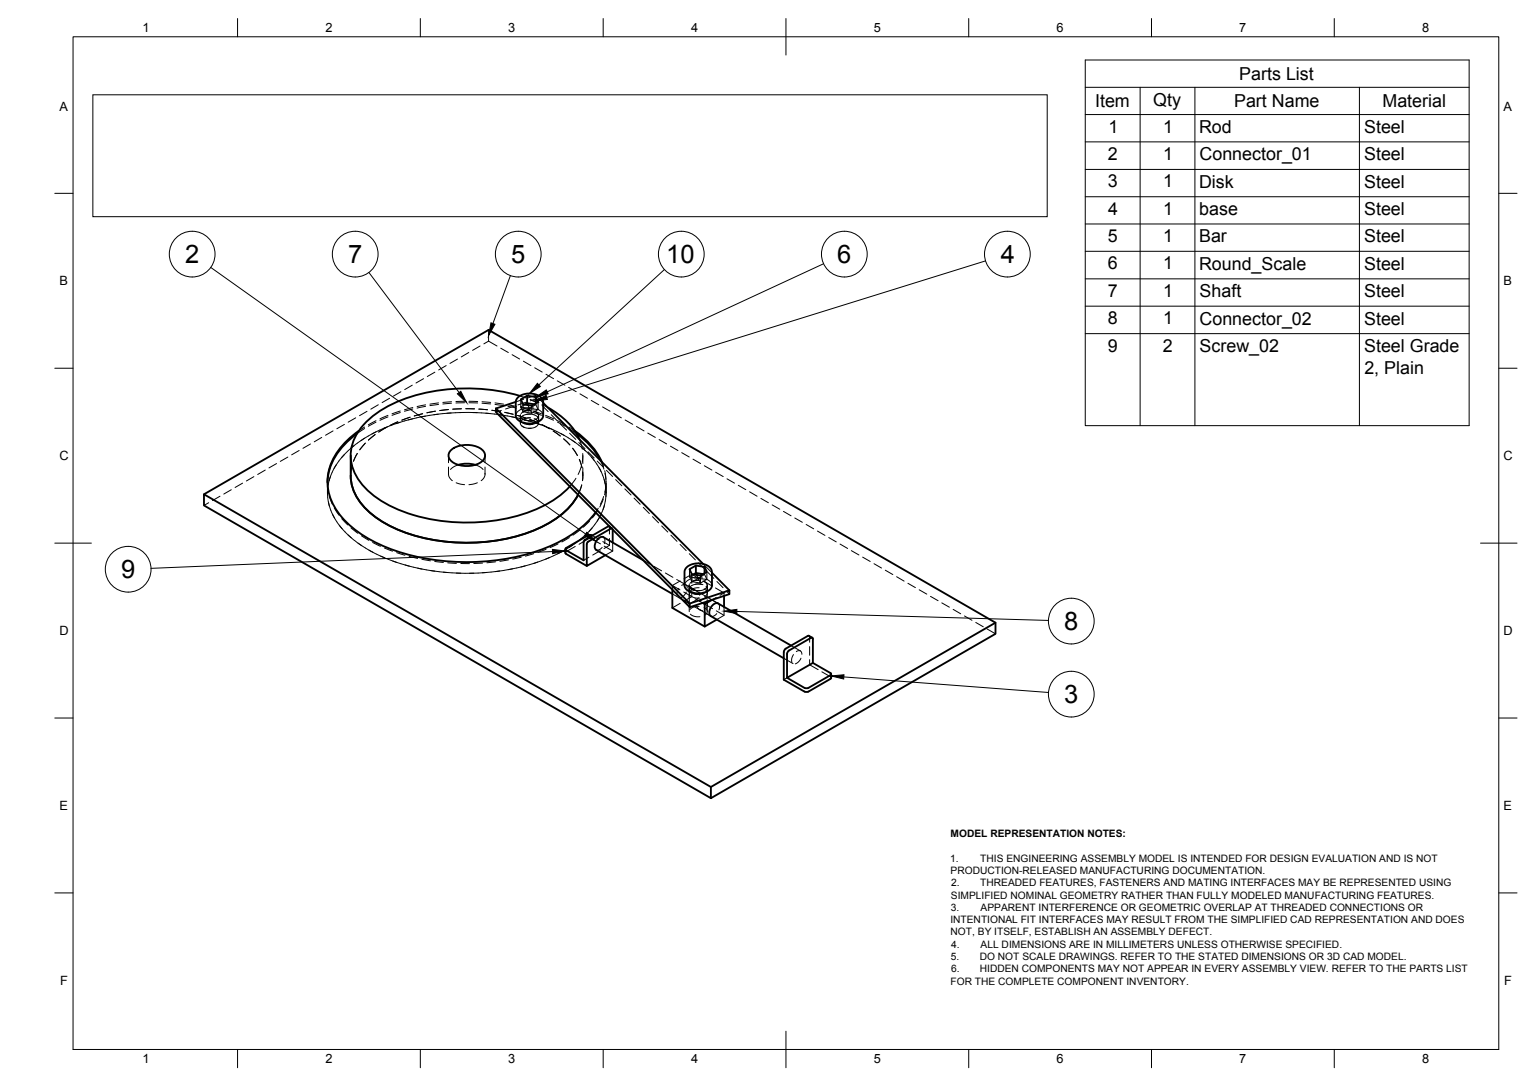
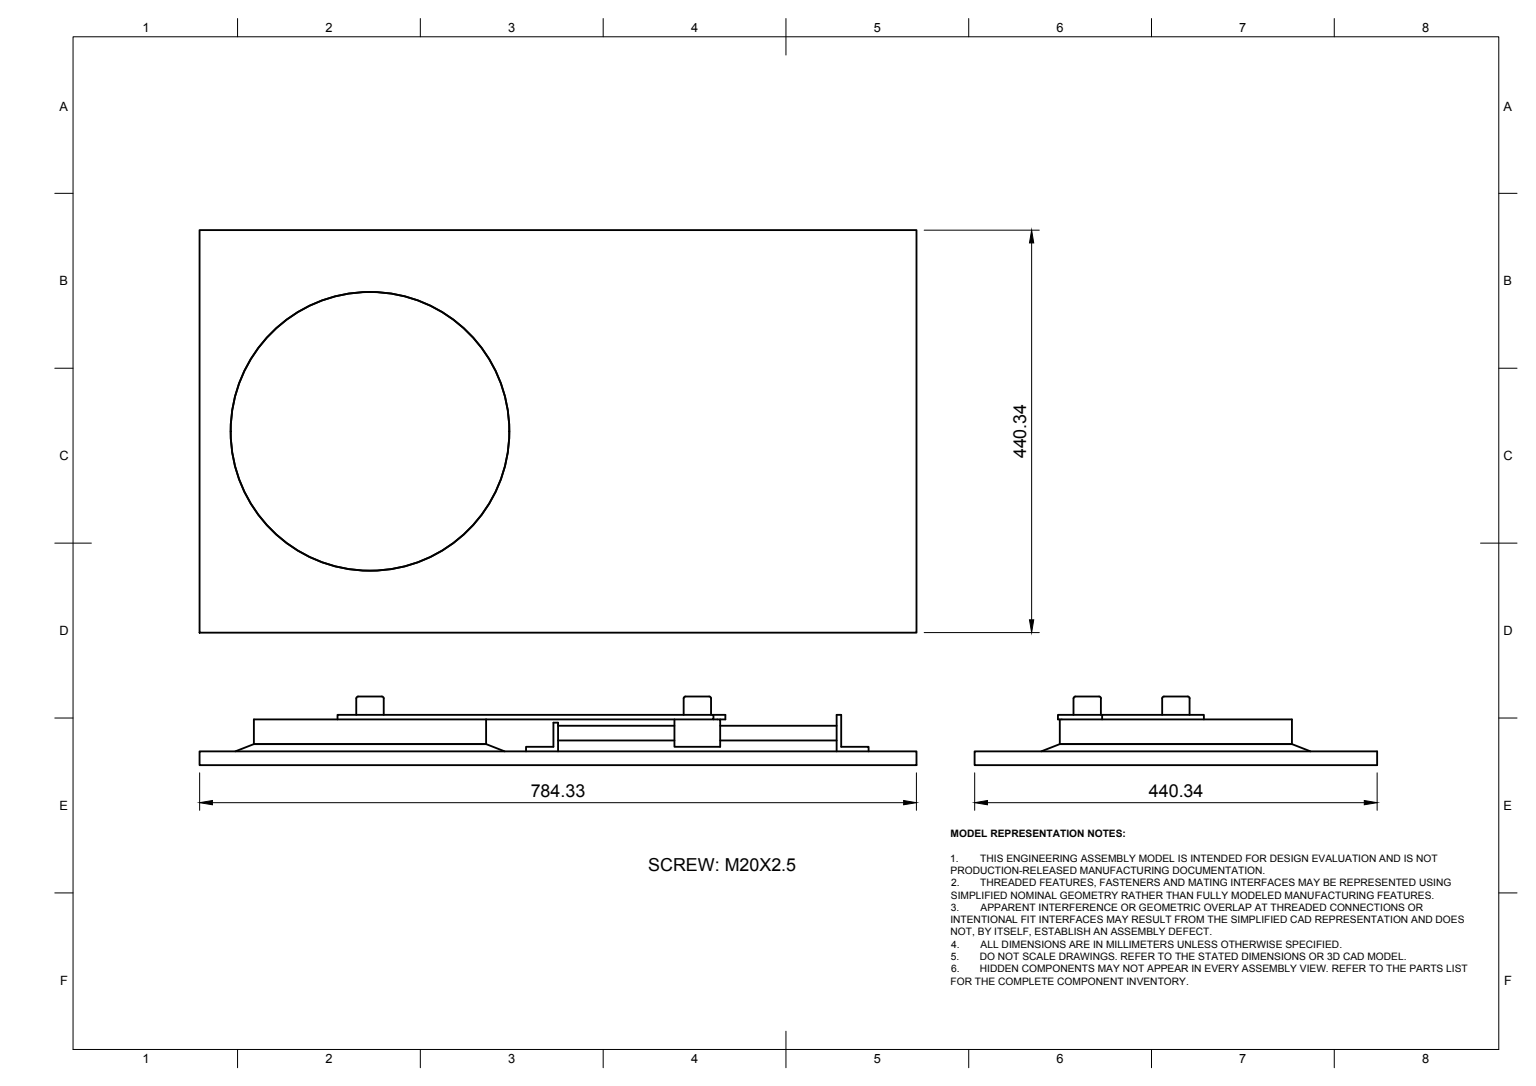
ISO-10303-21;
HEADER;
/* Generated by software containing ST-Developer
 * from STEP Tools, Inc. (www.steptools.com) 
 */

FILE_DESCRIPTION(
/* description */ (''),
/* implementation_level */ '2;1');

FILE_NAME(
/* name */ 'BR-205',
/* time_stamp */ '2026-10-05T19:45:59-07:00',
/* author */ (''),
/* organization */ (''),
/* preprocessor_version */ 'ST-DEVELOPER v20.2',
/* originating_system */ 'Autodesk Translation Framework v15.15.0.0',
/* authorisation */ '');

FILE_SCHEMA (('AUTOMOTIVE_DESIGN { 1 0 10303 214 3 1 1 }'));
ENDSEC;

DATA;
#10=MECHANICAL_DESIGN_GEOMETRIC_PRESENTATION_REPRESENTATION('',(#90,#91,
#92,#93,#94,#95,#96,#97,#98),#2462);
#11=ITEM_DEFINED_TRANSFORMATION($,$,#1437,#1569);
#12=ITEM_DEFINED_TRANSFORMATION($,$,#1443,#1570);
#13=ITEM_DEFINED_TRANSFORMATION($,$,#1464,#1571);
#14=ITEM_DEFINED_TRANSFORMATION($,$,#1478,#1572);
#15=ITEM_DEFINED_TRANSFORMATION($,$,#1488,#1573);
#16=ITEM_DEFINED_TRANSFORMATION($,$,#1501,#1574);
#17=ITEM_DEFINED_TRANSFORMATION($,$,#1509,#1575);
#18=ITEM_DEFINED_TRANSFORMATION($,$,#1523,#1576);
#19=ITEM_DEFINED_TRANSFORMATION($,$,#1544,#1577);
#20=ITEM_DEFINED_TRANSFORMATION($,$,#1544,#1578);
#21=(
REPRESENTATION_RELATIONSHIP($,$,#2498,#2497)
REPRESENTATION_RELATIONSHIP_WITH_TRANSFORMATION(#11)
SHAPE_REPRESENTATION_RELATIONSHIP()
);
#22=(
REPRESENTATION_RELATIONSHIP($,$,#2499,#2497)
REPRESENTATION_RELATIONSHIP_WITH_TRANSFORMATION(#12)
SHAPE_REPRESENTATION_RELATIONSHIP()
);
#23=(
REPRESENTATION_RELATIONSHIP($,$,#2500,#2497)
REPRESENTATION_RELATIONSHIP_WITH_TRANSFORMATION(#13)
SHAPE_REPRESENTATION_RELATIONSHIP()
);
#24=(
REPRESENTATION_RELATIONSHIP($,$,#2501,#2497)
REPRESENTATION_RELATIONSHIP_WITH_TRANSFORMATION(#14)
SHAPE_REPRESENTATION_RELATIONSHIP()
);
#25=(
REPRESENTATION_RELATIONSHIP($,$,#2502,#2497)
REPRESENTATION_RELATIONSHIP_WITH_TRANSFORMATION(#15)
SHAPE_REPRESENTATION_RELATIONSHIP()
);
#26=(
REPRESENTATION_RELATIONSHIP($,$,#2503,#2497)
REPRESENTATION_RELATIONSHIP_WITH_TRANSFORMATION(#16)
SHAPE_REPRESENTATION_RELATIONSHIP()
);
#27=(
REPRESENTATION_RELATIONSHIP($,$,#2504,#2497)
REPRESENTATION_RELATIONSHIP_WITH_TRANSFORMATION(#17)
SHAPE_REPRESENTATION_RELATIONSHIP()
);
#28=(
REPRESENTATION_RELATIONSHIP($,$,#2505,#2497)
REPRESENTATION_RELATIONSHIP_WITH_TRANSFORMATION(#18)
SHAPE_REPRESENTATION_RELATIONSHIP()
);
#29=(
REPRESENTATION_RELATIONSHIP($,$,#2506,#2497)
REPRESENTATION_RELATIONSHIP_WITH_TRANSFORMATION(#19)
SHAPE_REPRESENTATION_RELATIONSHIP()
);
#30=(
REPRESENTATION_RELATIONSHIP($,$,#2506,#2497)
REPRESENTATION_RELATIONSHIP_WITH_TRANSFORMATION(#20)
SHAPE_REPRESENTATION_RELATIONSHIP()
);
#31=CONTEXT_DEPENDENT_SHAPE_REPRESENTATION(#21,#2487);
#32=CONTEXT_DEPENDENT_SHAPE_REPRESENTATION(#22,#2488);
#33=CONTEXT_DEPENDENT_SHAPE_REPRESENTATION(#23,#2489);
#34=CONTEXT_DEPENDENT_SHAPE_REPRESENTATION(#24,#2490);
#35=CONTEXT_DEPENDENT_SHAPE_REPRESENTATION(#25,#2491);
#36=CONTEXT_DEPENDENT_SHAPE_REPRESENTATION(#26,#2492);
#37=CONTEXT_DEPENDENT_SHAPE_REPRESENTATION(#27,#2493);
#38=CONTEXT_DEPENDENT_SHAPE_REPRESENTATION(#28,#2494);
#39=CONTEXT_DEPENDENT_SHAPE_REPRESENTATION(#29,#2495);
#40=CONTEXT_DEPENDENT_SHAPE_REPRESENTATION(#30,#2496);
#41=NEXT_ASSEMBLY_USAGE_OCCURRENCE('Rod:1','Rod:1','Rod:1',#2508,#2509,
'Rod:1');
#42=NEXT_ASSEMBLY_USAGE_OCCURRENCE('Connector_01:1','Connector_01:1',
'Connector_01:1',#2508,#2510,'Connector_01:1');
#43=NEXT_ASSEMBLY_USAGE_OCCURRENCE('Disk:1','Disk:1','Disk:1',#2508,#2511,
'Disk:1');
#44=NEXT_ASSEMBLY_USAGE_OCCURRENCE('Base:1','Base:1','Base:1',#2508,#2512,
'Base:1');
#45=NEXT_ASSEMBLY_USAGE_OCCURRENCE('Bar:1','Bar:1','Bar:1',#2508,#2513,
'Bar:1');
#46=NEXT_ASSEMBLY_USAGE_OCCURRENCE('Round_Scale:1','Round_Scale:1',
'Round_Scale:1',#2508,#2514,'Round_Scale:1');
#47=NEXT_ASSEMBLY_USAGE_OCCURRENCE('Shaft:1','Shaft:1','Shaft:1',#2508,
#2515,'Shaft:1');
#48=NEXT_ASSEMBLY_USAGE_OCCURRENCE('Connector_02:1','Connector_02:1',
'Connector_02:1',#2508,#2516,'Connector_02:1');
#49=NEXT_ASSEMBLY_USAGE_OCCURRENCE('Screw_02:1','Screw_02:1',
'Screw_02:1',#2508,#2517,'Screw_02:1');
#50=NEXT_ASSEMBLY_USAGE_OCCURRENCE('Screw_02:2','Screw_02:2',
'Screw_02:2',#2508,#2517,'Screw_02:2');
#51=TOROIDAL_SURFACE('',#1547,13.,2.);
#52=B_SPLINE_CURVE_WITH_KNOTS('',3,(#2172,#2173,#2174,#2175,#2176,#2177,
#2178,#2179,#2180,#2181,#2182,#2183,#2184,#2185,#2186,#2187,#2188,#2189,
#2190,#2191,#2192,#2193),.UNSPECIFIED.,.F.,.F.,(4,2,2,2,2,2,2,2,2,2,4),
(1.29528463060384,1.61362869954164,1.93197276847945,2.26127101484344,2.42592013802544,
2.59056926120743,2.75521838438943,2.91986750757142,3.24916575393542,3.56750982287322,
3.88585389181102),.UNSPECIFIED.);
#53=B_SPLINE_CURVE_WITH_KNOTS('',3,(#2198,#2199,#2200,#2201,#2202,#2203,
#2204,#2205,#2206,#2207,#2208,#2209),.UNSPECIFIED.,.F.,.F.,(4,2,2,2,2,4),
(0.,0.164649123182026,0.329298246364052,0.658596492728105,0.976940561665974,
1.29528463060384),.UNSPECIFIED.);
#54=B_SPLINE_CURVE_WITH_KNOTS('',3,(#2210,#2211,#2212,#2213,#2214,#2215,
#2216,#2217,#2218,#2219,#2220,#2221),.UNSPECIFIED.,.F.,.F.,(4,2,2,2,2,4),
(3.88585389181102,4.20419796074889,4.52254202968676,4.85184027605081,5.01648939923284,
5.18113852241487),.UNSPECIFIED.);
#55=B_SPLINE_CURVE_WITH_KNOTS('',3,(#2223,#2224,#2225,#2226,#2227,#2228,
#2229,#2230,#2231,#2232,#2233,#2234,#2235,#2236,#2237,#2238,#2239,#2240,
#2241,#2242,#2243,#2244,#2245,#2246,#2247,#2248,#2249,#2250,#2251,#2252,
#2253,#2254,#2255,#2256,#2257,#2258,#2259,#2260,#2261,#2262,#2263,#2264),
 .UNSPECIFIED.,.T.,.F.,(4,2,2,2,2,2,2,2,2,2,2,2,2,2,2,2,2,2,2,2,4),(0.,
0.164649123182026,0.329298246364052,0.658596492728105,0.976940561665974,
1.29528463060384,1.61362869954165,1.93197276847945,2.26127101484344,2.42592013802544,
2.59056926120743,2.75521838438943,2.91986750757143,3.24916575393542,3.56750982287322,
3.88585389181102,4.20419796074889,4.52254202968676,4.85184027605081,5.01648939923284,
5.18113852241487),.UNSPECIFIED.);
#56=CONICAL_SURFACE('',#1505,139.7,1.19573207282673);
#57=FACE_BOUND('',#263,.T.);
#58=FACE_BOUND('',#264,.T.);
#59=FACE_BOUND('',#275,.T.);
#60=FACE_BOUND('',#277,.T.);
#61=FACE_BOUND('',#285,.T.);
#62=FACE_BOUND('',#286,.T.);
#63=FACE_BOUND('',#288,.T.);
#64=FACE_BOUND('',#289,.T.);
#65=FACE_BOUND('',#295,.T.);
#66=FACE_BOUND('',#298,.T.);
#67=FACE_BOUND('',#302,.T.);
#68=FACE_BOUND('',#305,.T.);
#69=FACE_BOUND('',#307,.T.);
#70=FACE_BOUND('',#323,.T.);
#71=FACE_BOUND('',#339,.T.);
#72=SHAPE_REPRESENTATION_RELATIONSHIP('SRR','None',#2498,#81);
#73=SHAPE_REPRESENTATION_RELATIONSHIP('SRR','None',#2499,#82);
#74=SHAPE_REPRESENTATION_RELATIONSHIP('SRR','None',#2500,#83);
#75=SHAPE_REPRESENTATION_RELATIONSHIP('SRR','None',#2501,#84);
#76=SHAPE_REPRESENTATION_RELATIONSHIP('SRR','None',#2502,#85);
#77=SHAPE_REPRESENTATION_RELATIONSHIP('SRR','None',#2503,#86);
#78=SHAPE_REPRESENTATION_RELATIONSHIP('SRR','None',#2504,#87);
#79=SHAPE_REPRESENTATION_RELATIONSHIP('SRR','None',#2505,#88);
#80=SHAPE_REPRESENTATION_RELATIONSHIP('SRR','None',#2506,#89);
#81=ADVANCED_BREP_SHAPE_REPRESENTATION('',(#99),#2453);
#82=ADVANCED_BREP_SHAPE_REPRESENTATION('',(#100),#2454);
#83=ADVANCED_BREP_SHAPE_REPRESENTATION('',(#101),#2455);
#84=ADVANCED_BREP_SHAPE_REPRESENTATION('',(#102),#2456);
#85=ADVANCED_BREP_SHAPE_REPRESENTATION('',(#103),#2457);
#86=ADVANCED_BREP_SHAPE_REPRESENTATION('',(#104),#2458);
#87=ADVANCED_BREP_SHAPE_REPRESENTATION('',(#105),#2459);
#88=ADVANCED_BREP_SHAPE_REPRESENTATION('',(#106),#2460);
#89=ADVANCED_BREP_SHAPE_REPRESENTATION('',(#107),#2461);
#90=STYLED_ITEM('',(#2552),#99);
#91=STYLED_ITEM('',(#2552),#100);
#92=STYLED_ITEM('',(#2553),#101);
#93=STYLED_ITEM('',(#2553),#102);
#94=STYLED_ITEM('',(#2552),#103);
#95=STYLED_ITEM('',(#2552),#104);
#96=STYLED_ITEM('',(#2552),#105);
#97=STYLED_ITEM('',(#2552),#106);
#98=STYLED_ITEM('',(#2552),#107);
#99=MANIFOLD_SOLID_BREP('Body1',#1327);
#100=MANIFOLD_SOLID_BREP('Body1',#1328);
#101=MANIFOLD_SOLID_BREP('Body1',#1329);
#102=MANIFOLD_SOLID_BREP('Body1',#1330);
#103=MANIFOLD_SOLID_BREP('Body1',#1331);
#104=MANIFOLD_SOLID_BREP('Body1',#1332);
#105=MANIFOLD_SOLID_BREP('Body1',#1333);
#106=MANIFOLD_SOLID_BREP('Body1',#1334);
#107=MANIFOLD_SOLID_BREP('Body1',#1335);
#108=PLANE('',#1441);
#109=PLANE('',#1442);
#110=PLANE('',#1447);
#111=PLANE('',#1449);
#112=PLANE('',#1455);
#113=PLANE('',#1456);
#114=PLANE('',#1460);
#115=PLANE('',#1461);
#116=PLANE('',#1462);
#117=PLANE('',#1463);
#118=PLANE('',#1468);
#119=PLANE('',#1469);
#120=PLANE('',#1474);
#121=PLANE('',#1477);
#122=PLANE('',#1482);
#123=PLANE('',#1483);
#124=PLANE('',#1484);
#125=PLANE('',#1485);
#126=PLANE('',#1486);
#127=PLANE('',#1487);
#128=PLANE('',#1495);
#129=PLANE('',#1496);
#130=PLANE('',#1497);
#131=PLANE('',#1498);
#132=PLANE('',#1499);
#133=PLANE('',#1500);
#134=PLANE('',#1507);
#135=PLANE('',#1508);
#136=PLANE('',#1515);
#137=PLANE('',#1518);
#138=PLANE('',#1519);
#139=PLANE('',#1520);
#140=PLANE('',#1521);
#141=PLANE('',#1522);
#142=PLANE('',#1527);
#143=PLANE('',#1528);
#144=PLANE('',#1532);
#145=PLANE('',#1536);
#146=PLANE('',#1538);
#147=PLANE('',#1541);
#148=PLANE('',#1542);
#149=PLANE('',#1543);
#150=PLANE('',#1545);
#151=PLANE('',#1551);
#152=PLANE('',#1554);
#153=PLANE('',#1555);
#154=PLANE('',#1556);
#155=PLANE('',#1557);
#156=PLANE('',#1558);
#157=PLANE('',#1559);
#158=PLANE('',#1560);
#159=PLANE('',#1561);
#160=PLANE('',#1562);
#161=PLANE('',#1563);
#162=PLANE('',#1564);
#163=PLANE('',#1565);
#164=PLANE('',#1568);
#165=FACE_OUTER_BOUND('',#245,.T.);
#166=FACE_OUTER_BOUND('',#246,.T.);
#167=FACE_OUTER_BOUND('',#247,.T.);
#168=FACE_OUTER_BOUND('',#248,.T.);
#169=FACE_OUTER_BOUND('',#249,.T.);
#170=FACE_OUTER_BOUND('',#250,.T.);
#171=FACE_OUTER_BOUND('',#251,.T.);
#172=FACE_OUTER_BOUND('',#252,.T.);
#173=FACE_OUTER_BOUND('',#253,.T.);
#174=FACE_OUTER_BOUND('',#254,.T.);
#175=FACE_OUTER_BOUND('',#255,.T.);
#176=FACE_OUTER_BOUND('',#256,.T.);
#177=FACE_OUTER_BOUND('',#257,.T.);
#178=FACE_OUTER_BOUND('',#258,.T.);
#179=FACE_OUTER_BOUND('',#259,.T.);
#180=FACE_OUTER_BOUND('',#260,.T.);
#181=FACE_OUTER_BOUND('',#261,.T.);
#182=FACE_OUTER_BOUND('',#262,.T.);
#183=FACE_OUTER_BOUND('',#265,.T.);
#184=FACE_OUTER_BOUND('',#266,.T.);
#185=FACE_OUTER_BOUND('',#267,.T.);
#186=FACE_OUTER_BOUND('',#268,.T.);
#187=FACE_OUTER_BOUND('',#269,.T.);
#188=FACE_OUTER_BOUND('',#270,.T.);
#189=FACE_OUTER_BOUND('',#271,.T.);
#190=FACE_OUTER_BOUND('',#272,.T.);
#191=FACE_OUTER_BOUND('',#273,.T.);
#192=FACE_OUTER_BOUND('',#274,.T.);
#193=FACE_OUTER_BOUND('',#276,.T.);
#194=FACE_OUTER_BOUND('',#278,.T.);
#195=FACE_OUTER_BOUND('',#279,.T.);
#196=FACE_OUTER_BOUND('',#280,.T.);
#197=FACE_OUTER_BOUND('',#281,.T.);
#198=FACE_OUTER_BOUND('',#282,.T.);
#199=FACE_OUTER_BOUND('',#283,.T.);
#200=FACE_OUTER_BOUND('',#284,.T.);
#201=FACE_OUTER_BOUND('',#287,.T.);
#202=FACE_OUTER_BOUND('',#290,.T.);
#203=FACE_OUTER_BOUND('',#291,.T.);
#204=FACE_OUTER_BOUND('',#292,.T.);
#205=FACE_OUTER_BOUND('',#293,.T.);
#206=FACE_OUTER_BOUND('',#294,.T.);
#207=FACE_OUTER_BOUND('',#296,.T.);
#208=FACE_OUTER_BOUND('',#297,.T.);
#209=FACE_OUTER_BOUND('',#299,.T.);
#210=FACE_OUTER_BOUND('',#300,.T.);
#211=FACE_OUTER_BOUND('',#301,.T.);
#212=FACE_OUTER_BOUND('',#303,.T.);
#213=FACE_OUTER_BOUND('',#304,.T.);
#214=FACE_OUTER_BOUND('',#306,.T.);
#215=FACE_OUTER_BOUND('',#308,.T.);
#216=FACE_OUTER_BOUND('',#309,.T.);
#217=FACE_OUTER_BOUND('',#310,.T.);
#218=FACE_OUTER_BOUND('',#311,.T.);
#219=FACE_OUTER_BOUND('',#312,.T.);
#220=FACE_OUTER_BOUND('',#313,.T.);
#221=FACE_OUTER_BOUND('',#314,.T.);
#222=FACE_OUTER_BOUND('',#315,.T.);
#223=FACE_OUTER_BOUND('',#316,.T.);
#224=FACE_OUTER_BOUND('',#317,.T.);
#225=FACE_OUTER_BOUND('',#318,.T.);
#226=FACE_OUTER_BOUND('',#319,.T.);
#227=FACE_OUTER_BOUND('',#320,.T.);
#228=FACE_OUTER_BOUND('',#321,.T.);
#229=FACE_OUTER_BOUND('',#322,.T.);
#230=FACE_OUTER_BOUND('',#324,.T.);
#231=FACE_OUTER_BOUND('',#325,.T.);
#232=FACE_OUTER_BOUND('',#326,.T.);
#233=FACE_OUTER_BOUND('',#327,.T.);
#234=FACE_OUTER_BOUND('',#328,.T.);
#235=FACE_OUTER_BOUND('',#329,.T.);
#236=FACE_OUTER_BOUND('',#330,.T.);
#237=FACE_OUTER_BOUND('',#331,.T.);
#238=FACE_OUTER_BOUND('',#332,.T.);
#239=FACE_OUTER_BOUND('',#333,.T.);
#240=FACE_OUTER_BOUND('',#334,.T.);
#241=FACE_OUTER_BOUND('',#335,.T.);
#242=FACE_OUTER_BOUND('',#336,.T.);
#243=FACE_OUTER_BOUND('',#337,.T.);
#244=FACE_OUTER_BOUND('',#338,.T.);
#245=EDGE_LOOP('',(#894,#895,#896,#897));
#246=EDGE_LOOP('',(#898));
#247=EDGE_LOOP('',(#899));
#248=EDGE_LOOP('',(#900,#901,#902,#903));
#249=EDGE_LOOP('',(#904,#905,#906,#907,#908,#909));
#250=EDGE_LOOP('',(#910,#911,#912,#913));
#251=EDGE_LOOP('',(#914,#915,#916,#917));
#252=EDGE_LOOP('',(#918,#919,#920,#921));
#253=EDGE_LOOP('',(#922,#923,#924,#925));
#254=EDGE_LOOP('',(#926,#927,#928,#929,#930,#931));
#255=EDGE_LOOP('',(#932,#933,#934,#935));
#256=EDGE_LOOP('',(#936,#937,#938,#939,#940,#941));
#257=EDGE_LOOP('',(#942,#943,#944,#945,#946,#947));
#258=EDGE_LOOP('',(#948,#949,#950,#951,#952,#953));
#259=EDGE_LOOP('',(#954,#955,#956,#957,#958,#959));
#260=EDGE_LOOP('',(#960,#961,#962,#963));
#261=EDGE_LOOP('',(#964));
#262=EDGE_LOOP('',(#965));
#263=EDGE_LOOP('',(#966));
#264=EDGE_LOOP('',(#967));
#265=EDGE_LOOP('',(#968,#969,#970,#971));
#266=EDGE_LOOP('',(#972));
#267=EDGE_LOOP('',(#973,#974,#975,#976));
#268=EDGE_LOOP('',(#977));
#269=EDGE_LOOP('',(#978,#979,#980,#981));
#270=EDGE_LOOP('',(#982,#983,#984,#985));
#271=EDGE_LOOP('',(#986,#987,#988,#989));
#272=EDGE_LOOP('',(#990,#991,#992,#993));
#273=EDGE_LOOP('',(#994,#995,#996,#997));
#274=EDGE_LOOP('',(#998,#999,#1000,#1001));
#275=EDGE_LOOP('',(#1002));
#276=EDGE_LOOP('',(#1003,#1004,#1005,#1006));
#277=EDGE_LOOP('',(#1007));
#278=EDGE_LOOP('',(#1008,#1009,#1010,#1011));
#279=EDGE_LOOP('',(#1012,#1013,#1014,#1015));
#280=EDGE_LOOP('',(#1016,#1017,#1018,#1019));
#281=EDGE_LOOP('',(#1020,#1021,#1022,#1023));
#282=EDGE_LOOP('',(#1024,#1025,#1026,#1027));
#283=EDGE_LOOP('',(#1028,#1029,#1030,#1031));
#284=EDGE_LOOP('',(#1032,#1033,#1034,#1035));
#285=EDGE_LOOP('',(#1036));
#286=EDGE_LOOP('',(#1037));
#287=EDGE_LOOP('',(#1038,#1039,#1040,#1041));
#288=EDGE_LOOP('',(#1042));
#289=EDGE_LOOP('',(#1043));
#290=EDGE_LOOP('',(#1044,#1045,#1046,#1047));
#291=EDGE_LOOP('',(#1048,#1049,#1050,#1051));
#292=EDGE_LOOP('',(#1052));
#293=EDGE_LOOP('',(#1053));
#294=EDGE_LOOP('',(#1054,#1055,#1056,#1057,#1058,#1059,#1060,#1061,#1062));
#295=EDGE_LOOP('',(#1063));
#296=EDGE_LOOP('',(#1064,#1065,#1066,#1067,#1068,#1069));
#297=EDGE_LOOP('',(#1070,#1071,#1072,#1073));
#298=EDGE_LOOP('',(#1074));
#299=EDGE_LOOP('',(#1075,#1076,#1077,#1078));
#300=EDGE_LOOP('',(#1079,#1080,#1081,#1082));
#301=EDGE_LOOP('',(#1083,#1084,#1085,#1086));
#302=EDGE_LOOP('',(#1087));
#303=EDGE_LOOP('',(#1088,#1089,#1090,#1091));
#304=EDGE_LOOP('',(#1092,#1093,#1094,#1095));
#305=EDGE_LOOP('',(#1096));
#306=EDGE_LOOP('',(#1097,#1098,#1099,#1100));
#307=EDGE_LOOP('',(#1101));
#308=EDGE_LOOP('',(#1102,#1103,#1104,#1105));
#309=EDGE_LOOP('',(#1106,#1107,#1108,#1109));
#310=EDGE_LOOP('',(#1110,#1111,#1112,#1113,#1114,#1115));
#311=EDGE_LOOP('',(#1116,#1117,#1118,#1119));
#312=EDGE_LOOP('',(#1120,#1121,#1122,#1123,#1124,#1125));
#313=EDGE_LOOP('',(#1126,#1127,#1128,#1129));
#314=EDGE_LOOP('',(#1130,#1131,#1132,#1133,#1134,#1135));
#315=EDGE_LOOP('',(#1136,#1137,#1138,#1139));
#316=EDGE_LOOP('',(#1140,#1141,#1142,#1143));
#317=EDGE_LOOP('',(#1144,#1145,#1146,#1147,#1148,#1149));
#318=EDGE_LOOP('',(#1150,#1151,#1152,#1153,#1154,#1155));
#319=EDGE_LOOP('',(#1156,#1157,#1158,#1159,#1160,#1161));
#320=EDGE_LOOP('',(#1162));
#321=EDGE_LOOP('',(#1163,#1164,#1165,#1166));
#322=EDGE_LOOP('',(#1167));
#323=EDGE_LOOP('',(#1168,#1169,#1170,#1171,#1172,#1173));
#324=EDGE_LOOP('',(#1174,#1175,#1176,#1177));
#325=EDGE_LOOP('',(#1178,#1179,#1180));
#326=EDGE_LOOP('',(#1181,#1182,#1183));
#327=EDGE_LOOP('',(#1184,#1185,#1186));
#328=EDGE_LOOP('',(#1187,#1188,#1189));
#329=EDGE_LOOP('',(#1190,#1191,#1192));
#330=EDGE_LOOP('',(#1193,#1194,#1195));
#331=EDGE_LOOP('',(#1196,#1197,#1198,#1199));
#332=EDGE_LOOP('',(#1200,#1201,#1202,#1203));
#333=EDGE_LOOP('',(#1204,#1205,#1206,#1207));
#334=EDGE_LOOP('',(#1208,#1209,#1210,#1211));
#335=EDGE_LOOP('',(#1212,#1213,#1214,#1215));
#336=EDGE_LOOP('',(#1216,#1217,#1218,#1219));
#337=EDGE_LOOP('',(#1220,#1221,#1222,#1223));
#338=EDGE_LOOP('',(#1224));
#339=EDGE_LOOP('',(#1225));
#340=LINE('',#1990,#459);
#341=LINE('',#2000,#460);
#342=LINE('',#2003,#461);
#343=LINE('',#2006,#462);
#344=LINE('',#2010,#463);
#345=LINE('',#2012,#464);
#346=LINE('',#2013,#465);
#347=LINE('',#2016,#466);
#348=LINE('',#2017,#467);
#349=LINE('',#2021,#468);
#350=LINE('',#2027,#469);
#351=LINE('',#2030,#470);
#352=LINE('',#2033,#471);
#353=LINE('',#2035,#472);
#354=LINE('',#2036,#473);
#355=LINE('',#2039,#474);
#356=LINE('',#2041,#475);
#357=LINE('',#2043,#476);
#358=LINE('',#2048,#477);
#359=LINE('',#2050,#478);
#360=LINE('',#2051,#479);
#361=LINE('',#2053,#480);
#362=LINE('',#2055,#481);
#363=LINE('',#2062,#482);
#364=LINE('',#2072,#483);
#365=LINE('',#2077,#484);
#366=LINE('',#2085,#485);
#367=LINE('',#2090,#486);
#368=LINE('',#2092,#487);
#369=LINE('',#2094,#488);
#370=LINE('',#2095,#489);
#371=LINE('',#2098,#490);
#372=LINE('',#2100,#491);
#373=LINE('',#2101,#492);
#374=LINE('',#2104,#493);
#375=LINE('',#2106,#494);
#376=LINE('',#2107,#495);
#377=LINE('',#2109,#496);
#378=LINE('',#2110,#497);
#379=LINE('',#2118,#498);
#380=LINE('',#2124,#499);
#381=LINE('',#2129,#500);
#382=LINE('',#2131,#501);
#383=LINE('',#2133,#502);
#384=LINE('',#2134,#503);
#385=LINE('',#2137,#504);
#386=LINE('',#2139,#505);
#387=LINE('',#2140,#506);
#388=LINE('',#2143,#507);
#389=LINE('',#2145,#508);
#390=LINE('',#2146,#509);
#391=LINE('',#2148,#510);
#392=LINE('',#2149,#511);
#393=LINE('',#2157,#512);
#394=LINE('',#2161,#513);
#395=LINE('',#2170,#514);
#396=LINE('',#2195,#515);
#397=LINE('',#2268,#516);
#398=LINE('',#2272,#517);
#399=LINE('',#2274,#518);
#400=LINE('',#2276,#519);
#401=LINE('',#2277,#520);
#402=LINE('',#2280,#521);
#403=LINE('',#2284,#522);
#404=LINE('',#2286,#523);
#405=LINE('',#2287,#524);
#406=LINE('',#2290,#525);
#407=LINE('',#2291,#526);
#408=LINE('',#2294,#527);
#409=LINE('',#2295,#528);
#410=LINE('',#2297,#529);
#411=LINE('',#2305,#530);
#412=LINE('',#2308,#531);
#413=LINE('',#2311,#532);
#414=LINE('',#2313,#533);
#415=LINE('',#2314,#534);
#416=LINE('',#2317,#535);
#417=LINE('',#2319,#536);
#418=LINE('',#2321,#537);
#419=LINE('',#2325,#538);
#420=LINE('',#2329,#539);
#421=LINE('',#2331,#540);
#422=LINE('',#2333,#541);
#423=LINE('',#2334,#542);
#424=LINE('',#2340,#543);
#425=LINE('',#2343,#544);
#426=LINE('',#2345,#545);
#427=LINE('',#2348,#546);
#428=LINE('',#2351,#547);
#429=LINE('',#2352,#548);
#430=LINE('',#2357,#549);
#431=LINE('',#2358,#550);
#432=LINE('',#2360,#551);
#433=LINE('',#2375,#552);
#434=LINE('',#2377,#553);
#435=LINE('',#2379,#554);
#436=LINE('',#2381,#555);
#437=LINE('',#2383,#556);
#438=LINE('',#2384,#557);
#439=LINE('',#2388,#558);
#440=LINE('',#2392,#559);
#441=LINE('',#2394,#560);
#442=LINE('',#2395,#561);
#443=LINE('',#2398,#562);
#444=LINE('',#2399,#563);
#445=LINE('',#2402,#564);
#446=LINE('',#2403,#565);
#447=LINE('',#2406,#566);
#448=LINE('',#2407,#567);
#449=LINE('',#2410,#568);
#450=LINE('',#2411,#569);
#451=LINE('',#2413,#570);
#452=LINE('',#2415,#571);
#453=LINE('',#2416,#572);
#454=LINE('',#2418,#573);
#455=LINE('',#2420,#574);
#456=LINE('',#2422,#575);
#457=LINE('',#2424,#576);
#458=LINE('',#2428,#577);
#459=VECTOR('',#1587,8.);
#460=VECTOR('',#1600,10.);
#461=VECTOR('',#1603,10.);
#462=VECTOR('',#1606,10.);
#463=VECTOR('',#1609,10.);
#464=VECTOR('',#1610,10.);
#465=VECTOR('',#1611,10.);
#466=VECTOR('',#1614,10.);
#467=VECTOR('',#1615,10.);
#468=VECTOR('',#1620,10.);
#469=VECTOR('',#1625,10.);
#470=VECTOR('',#1628,10.);
#471=VECTOR('',#1631,10.);
#472=VECTOR('',#1632,10.);
#473=VECTOR('',#1633,10.);
#474=VECTOR('',#1636,10.);
#475=VECTOR('',#1637,10.);
#476=VECTOR('',#1638,10.);
#477=VECTOR('',#1645,10.);
#478=VECTOR('',#1648,10.);
#479=VECTOR('',#1649,10.);
#480=VECTOR('',#1652,10.);
#481=VECTOR('',#1655,10.);
#482=VECTOR('',#1664,10.);
#483=VECTOR('',#1677,20.);
#484=VECTOR('',#1684,127.);
#485=VECTOR('',#1695,152.4);
#486=VECTOR('',#1700,10.);
#487=VECTOR('',#1701,10.);
#488=VECTOR('',#1702,10.);
#489=VECTOR('',#1703,10.);
#490=VECTOR('',#1706,10.);
#491=VECTOR('',#1707,10.);
#492=VECTOR('',#1708,10.);
#493=VECTOR('',#1711,10.);
#494=VECTOR('',#1712,10.);
#495=VECTOR('',#1713,10.);
#496=VECTOR('',#1716,10.);
#497=VECTOR('',#1717,10.);
#498=VECTOR('',#1728,10.);
#499=VECTOR('',#1735,10.);
#500=VECTOR('',#1740,10.);
#501=VECTOR('',#1741,10.);
#502=VECTOR('',#1742,10.);
#503=VECTOR('',#1743,10.);
#504=VECTOR('',#1746,10.);
#505=VECTOR('',#1747,10.);
#506=VECTOR('',#1748,10.);
#507=VECTOR('',#1751,10.);
#508=VECTOR('',#1752,10.);
#509=VECTOR('',#1753,10.);
#510=VECTOR('',#1756,10.);
#511=VECTOR('',#1757,10.);
#512=VECTOR('',#1768,152.4);
#513=VECTOR('',#1773,139.7);
#514=VECTOR('',#1786,9.89525);
#515=VECTOR('',#1787,9.89525);
#516=VECTOR('',#1794,8.);
#517=VECTOR('',#1797,10.);
#518=VECTOR('',#1798,10.);
#519=VECTOR('',#1799,10.);
#520=VECTOR('',#1800,10.);
#521=VECTOR('',#1803,8.);
#522=VECTOR('',#1808,10.);
#523=VECTOR('',#1809,10.);
#524=VECTOR('',#1810,10.);
#525=VECTOR('',#1813,10.);
#526=VECTOR('',#1814,10.);
#527=VECTOR('',#1817,10.);
#528=VECTOR('',#1818,10.);
#529=VECTOR('',#1821,10.);
#530=VECTOR('',#1830,10.);
#531=VECTOR('',#1833,10.);
#532=VECTOR('',#1836,10.);
#533=VECTOR('',#1837,10.);
#534=VECTOR('',#1838,10.);
#535=VECTOR('',#1841,10.);
#536=VECTOR('',#1842,10.);
#537=VECTOR('',#1843,10.);
#538=VECTOR('',#1848,10.);
#539=VECTOR('',#1853,10.);
#540=VECTOR('',#1854,10.);
#541=VECTOR('',#1855,10.);
#542=VECTOR('',#1856,10.);
#543=VECTOR('',#1861,10.);
#544=VECTOR('',#1864,10.);
#545=VECTOR('',#1867,10.);
#546=VECTOR('',#1870,10.);
#547=VECTOR('',#1873,10.);
#548=VECTOR('',#1874,10.);
#549=VECTOR('',#1881,10.);
#550=VECTOR('',#1882,10.);
#551=VECTOR('',#1885,10.);
#552=VECTOR('',#1904,10.);
#553=VECTOR('',#1905,10.);
#554=VECTOR('',#1906,10.);
#555=VECTOR('',#1907,10.);
#556=VECTOR('',#1908,10.);
#557=VECTOR('',#1909,10.);
#558=VECTOR('',#1914,15.);
#559=VECTOR('',#1917,9.99999999999999);
#560=VECTOR('',#1918,10.);
#561=VECTOR('',#1919,10.);
#562=VECTOR('',#1922,10.);
#563=VECTOR('',#1923,10.);
#564=VECTOR('',#1926,10.);
#565=VECTOR('',#1927,9.99999999999999);
#566=VECTOR('',#1930,10.);
#567=VECTOR('',#1931,10.);
#568=VECTOR('',#1934,10.);
#569=VECTOR('',#1935,10.);
#570=VECTOR('',#1938,9.99999999999999);
#571=VECTOR('',#1941,10.);
#572=VECTOR('',#1942,10.);
#573=VECTOR('',#1945,10.);
#574=VECTOR('',#1948,10.);
#575=VECTOR('',#1951,10.);
#576=VECTOR('',#1954,10.);
#577=VECTOR('',#1959,9.89525);
#578=CIRCLE('',#1439,8.);
#579=CIRCLE('',#1440,8.);
#580=CIRCLE('',#1445,3.);
#581=CIRCLE('',#1446,3.);
#582=CIRCLE('',#1448,3.);
#583=CIRCLE('',#1451,3.);
#584=CIRCLE('',#1453,3.);
#585=CIRCLE('',#1454,3.);
#586=CIRCLE('',#1457,3.);
#587=CIRCLE('',#1459,3.);
#588=CIRCLE('',#1466,10.);
#589=CIRCLE('',#1467,10.);
#590=CIRCLE('',#1470,127.);
#591=CIRCLE('',#1471,20.);
#592=CIRCLE('',#1473,20.);
#593=CIRCLE('',#1476,127.);
#594=CIRCLE('',#1480,152.4);
#595=CIRCLE('',#1481,152.4);
#596=CIRCLE('',#1490,10.);
#597=CIRCLE('',#1491,10.);
#598=CIRCLE('',#1493,10.);
#599=CIRCLE('',#1494,10.);
#600=CIRCLE('',#1503,152.4);
#601=CIRCLE('',#1504,152.4);
#602=CIRCLE('',#1506,127.);
#603=CIRCLE('',#1511,9.89525);
#604=CIRCLE('',#1512,9.89525);
#605=CIRCLE('',#1514,8.);
#606=CIRCLE('',#1517,8.);
#607=CIRCLE('',#1525,2.);
#608=CIRCLE('',#1526,2.);
#609=CIRCLE('',#1529,2.);
#610=CIRCLE('',#1531,2.);
#611=CIRCLE('',#1534,3.);
#612=CIRCLE('',#1535,3.);
#613=CIRCLE('',#1537,3.);
#614=CIRCLE('',#1540,3.);
#615=CIRCLE('',#1546,9.89525);
#616=CIRCLE('',#1548,15.);
#617=CIRCLE('',#1549,2.);
#618=CIRCLE('',#1550,13.);
#619=CIRCLE('',#1553,15.);
#620=CIRCLE('',#1567,9.89525);
#621=VERTEX_POINT('',#1987);
#622=VERTEX_POINT('',#1989);
#623=VERTEX_POINT('',#1996);
#624=VERTEX_POINT('',#1997);
#625=VERTEX_POINT('',#1999);
#626=VERTEX_POINT('',#2001);
#627=VERTEX_POINT('',#2005);
#628=VERTEX_POINT('',#2007);
#629=VERTEX_POINT('',#2009);
#630=VERTEX_POINT('',#2011);
#631=VERTEX_POINT('',#2015);
#632=VERTEX_POINT('',#2019);
#633=VERTEX_POINT('',#2023);
#634=VERTEX_POINT('',#2024);
#635=VERTEX_POINT('',#2026);
#636=VERTEX_POINT('',#2028);
#637=VERTEX_POINT('',#2032);
#638=VERTEX_POINT('',#2034);
#639=VERTEX_POINT('',#2038);
#640=VERTEX_POINT('',#2040);
#641=VERTEX_POINT('',#2042);
#642=VERTEX_POINT('',#2046);
#643=VERTEX_POINT('',#2059);
#644=VERTEX_POINT('',#2061);
#645=VERTEX_POINT('',#2066);
#646=VERTEX_POINT('',#2068);
#647=VERTEX_POINT('',#2071);
#648=VERTEX_POINT('',#2076);
#649=VERTEX_POINT('',#2082);
#650=VERTEX_POINT('',#2084);
#651=VERTEX_POINT('',#2088);
#652=VERTEX_POINT('',#2089);
#653=VERTEX_POINT('',#2091);
#654=VERTEX_POINT('',#2093);
#655=VERTEX_POINT('',#2097);
#656=VERTEX_POINT('',#2099);
#657=VERTEX_POINT('',#2103);
#658=VERTEX_POINT('',#2105);
#659=VERTEX_POINT('',#2115);
#660=VERTEX_POINT('',#2117);
#661=VERTEX_POINT('',#2121);
#662=VERTEX_POINT('',#2123);
#663=VERTEX_POINT('',#2127);
#664=VERTEX_POINT('',#2128);
#665=VERTEX_POINT('',#2130);
#666=VERTEX_POINT('',#2132);
#667=VERTEX_POINT('',#2136);
#668=VERTEX_POINT('',#2138);
#669=VERTEX_POINT('',#2142);
#670=VERTEX_POINT('',#2144);
#671=VERTEX_POINT('',#2154);
#672=VERTEX_POINT('',#2156);
#673=VERTEX_POINT('',#2160);
#674=VERTEX_POINT('',#2167);
#675=VERTEX_POINT('',#2169);
#676=VERTEX_POINT('',#2171);
#677=VERTEX_POINT('',#2194);
#678=VERTEX_POINT('',#2197);
#679=VERTEX_POINT('',#2222);
#680=VERTEX_POINT('',#2266);
#681=VERTEX_POINT('',#2270);
#682=VERTEX_POINT('',#2271);
#683=VERTEX_POINT('',#2273);
#684=VERTEX_POINT('',#2275);
#685=VERTEX_POINT('',#2279);
#686=VERTEX_POINT('',#2283);
#687=VERTEX_POINT('',#2285);
#688=VERTEX_POINT('',#2289);
#689=VERTEX_POINT('',#2293);
#690=VERTEX_POINT('',#2301);
#691=VERTEX_POINT('',#2302);
#692=VERTEX_POINT('',#2304);
#693=VERTEX_POINT('',#2306);
#694=VERTEX_POINT('',#2310);
#695=VERTEX_POINT('',#2312);
#696=VERTEX_POINT('',#2316);
#697=VERTEX_POINT('',#2318);
#698=VERTEX_POINT('',#2320);
#699=VERTEX_POINT('',#2324);
#700=VERTEX_POINT('',#2328);
#701=VERTEX_POINT('',#2330);
#702=VERTEX_POINT('',#2332);
#703=VERTEX_POINT('',#2336);
#704=VERTEX_POINT('',#2337);
#705=VERTEX_POINT('',#2339);
#706=VERTEX_POINT('',#2341);
#707=VERTEX_POINT('',#2346);
#708=VERTEX_POINT('',#2350);
#709=VERTEX_POINT('',#2356);
#710=VERTEX_POINT('',#2364);
#711=VERTEX_POINT('',#2367);
#712=VERTEX_POINT('',#2369);
#713=VERTEX_POINT('',#2373);
#714=VERTEX_POINT('',#2374);
#715=VERTEX_POINT('',#2376);
#716=VERTEX_POINT('',#2378);
#717=VERTEX_POINT('',#2380);
#718=VERTEX_POINT('',#2382);
#719=VERTEX_POINT('',#2386);
#720=VERTEX_POINT('',#2390);
#721=VERTEX_POINT('',#2391);
#722=VERTEX_POINT('',#2393);
#723=VERTEX_POINT('',#2397);
#724=VERTEX_POINT('',#2401);
#725=VERTEX_POINT('',#2405);
#726=VERTEX_POINT('',#2409);
#727=VERTEX_POINT('',#2427);
#728=EDGE_CURVE('',#621,#621,#578,.T.);
#729=EDGE_CURVE('',#621,#622,#340,.T.);
#730=EDGE_CURVE('',#622,#622,#579,.T.);
#731=EDGE_CURVE('',#623,#624,#580,.T.);
#732=EDGE_CURVE('',#624,#625,#341,.T.);
#733=EDGE_CURVE('',#625,#626,#581,.T.);
#734=EDGE_CURVE('',#626,#623,#342,.T.);
#735=EDGE_CURVE('',#627,#625,#343,.T.);
#736=EDGE_CURVE('',#628,#627,#582,.T.);
#737=EDGE_CURVE('',#629,#628,#344,.T.);
#738=EDGE_CURVE('',#629,#630,#345,.T.);
#739=EDGE_CURVE('',#630,#626,#346,.T.);
#740=EDGE_CURVE('',#624,#631,#347,.T.);
#741=EDGE_CURVE('',#627,#631,#348,.T.);
#742=EDGE_CURVE('',#631,#632,#583,.T.);
#743=EDGE_CURVE('',#632,#628,#349,.T.);
#744=EDGE_CURVE('',#633,#634,#584,.T.);
#745=EDGE_CURVE('',#634,#635,#350,.T.);
#746=EDGE_CURVE('',#635,#636,#585,.T.);
#747=EDGE_CURVE('',#636,#633,#351,.T.);
#748=EDGE_CURVE('',#637,#636,#352,.T.);
#749=EDGE_CURVE('',#638,#637,#353,.T.);
#750=EDGE_CURVE('',#633,#638,#354,.T.);
#751=EDGE_CURVE('',#639,#635,#355,.T.);
#752=EDGE_CURVE('',#640,#639,#356,.T.);
#753=EDGE_CURVE('',#641,#640,#357,.T.);
#754=EDGE_CURVE('',#637,#641,#586,.T.);
#755=EDGE_CURVE('',#642,#638,#587,.T.);
#756=EDGE_CURVE('',#641,#642,#358,.T.);
#757=EDGE_CURVE('',#642,#630,#359,.T.);
#758=EDGE_CURVE('',#629,#634,#360,.T.);
#759=EDGE_CURVE('',#639,#632,#361,.T.);
#760=EDGE_CURVE('',#640,#623,#362,.T.);
#761=EDGE_CURVE('',#643,#643,#588,.T.);
#762=EDGE_CURVE('',#643,#644,#363,.T.);
#763=EDGE_CURVE('',#644,#644,#589,.T.);
#764=EDGE_CURVE('',#645,#645,#590,.T.);
#765=EDGE_CURVE('',#646,#646,#591,.T.);
#766=EDGE_CURVE('',#646,#647,#364,.T.);
#767=EDGE_CURVE('',#647,#647,#592,.T.);
#768=EDGE_CURVE('',#645,#648,#365,.T.);
#769=EDGE_CURVE('',#648,#648,#593,.F.);
#770=EDGE_CURVE('',#649,#649,#594,.T.);
#771=EDGE_CURVE('',#649,#650,#366,.T.);
#772=EDGE_CURVE('',#650,#650,#595,.T.);
#773=EDGE_CURVE('',#651,#652,#367,.T.);
#774=EDGE_CURVE('',#652,#653,#368,.T.);
#775=EDGE_CURVE('',#654,#653,#369,.T.);
#776=EDGE_CURVE('',#651,#654,#370,.T.);
#777=EDGE_CURVE('',#655,#651,#371,.T.);
#778=EDGE_CURVE('',#656,#654,#372,.T.);
#779=EDGE_CURVE('',#655,#656,#373,.T.);
#780=EDGE_CURVE('',#657,#655,#374,.T.);
#781=EDGE_CURVE('',#658,#656,#375,.T.);
#782=EDGE_CURVE('',#657,#658,#376,.T.);
#783=EDGE_CURVE('',#652,#657,#377,.T.);
#784=EDGE_CURVE('',#653,#658,#378,.T.);
#785=EDGE_CURVE('',#659,#659,#596,.T.);
#786=EDGE_CURVE('',#659,#660,#379,.T.);
#787=EDGE_CURVE('',#660,#660,#597,.T.);
#788=EDGE_CURVE('',#661,#661,#598,.T.);
#789=EDGE_CURVE('',#661,#662,#380,.T.);
#790=EDGE_CURVE('',#662,#662,#599,.T.);
#791=EDGE_CURVE('',#663,#664,#381,.T.);
#792=EDGE_CURVE('',#663,#665,#382,.F.);
#793=EDGE_CURVE('',#666,#665,#383,.T.);
#794=EDGE_CURVE('',#664,#666,#384,.T.);
#795=EDGE_CURVE('',#667,#664,#385,.F.);
#796=EDGE_CURVE('',#668,#666,#386,.F.);
#797=EDGE_CURVE('',#667,#668,#387,.F.);
#798=EDGE_CURVE('',#669,#667,#388,.T.);
#799=EDGE_CURVE('',#670,#668,#389,.T.);
#800=EDGE_CURVE('',#669,#670,#390,.T.);
#801=EDGE_CURVE('',#663,#669,#391,.F.);
#802=EDGE_CURVE('',#665,#670,#392,.F.);
#803=EDGE_CURVE('',#671,#671,#600,.T.);
#804=EDGE_CURVE('',#671,#672,#393,.T.);
#805=EDGE_CURVE('',#672,#672,#601,.F.);
#806=EDGE_CURVE('',#671,#673,#394,.T.);
#807=EDGE_CURVE('',#673,#673,#602,.T.);
#808=EDGE_CURVE('',#674,#674,#603,.T.);
#809=EDGE_CURVE('',#674,#675,#395,.T.);
#810=EDGE_CURVE('',#676,#675,#52,.T.);
#811=EDGE_CURVE('',#676,#677,#396,.T.);
#812=EDGE_CURVE('',#677,#677,#604,.T.);
#813=EDGE_CURVE('',#678,#676,#53,.T.);
#814=EDGE_CURVE('',#675,#678,#54,.T.);
#815=EDGE_CURVE('',#679,#679,#55,.T.);
#816=EDGE_CURVE('',#680,#680,#605,.T.);
#817=EDGE_CURVE('',#680,#678,#397,.T.);
#818=EDGE_CURVE('',#681,#682,#398,.T.);
#819=EDGE_CURVE('',#682,#683,#399,.T.);
#820=EDGE_CURVE('',#683,#684,#400,.T.);
#821=EDGE_CURVE('',#684,#681,#401,.T.);
#822=EDGE_CURVE('',#679,#685,#402,.T.);
#823=EDGE_CURVE('',#685,#685,#606,.T.);
#824=EDGE_CURVE('',#686,#682,#403,.T.);
#825=EDGE_CURVE('',#687,#686,#404,.T.);
#826=EDGE_CURVE('',#683,#687,#405,.T.);
#827=EDGE_CURVE('',#688,#687,#406,.T.);
#828=EDGE_CURVE('',#684,#688,#407,.T.);
#829=EDGE_CURVE('',#689,#688,#408,.T.);
#830=EDGE_CURVE('',#681,#689,#409,.T.);
#831=EDGE_CURVE('',#686,#689,#410,.T.);
#832=EDGE_CURVE('',#690,#691,#607,.T.);
#833=EDGE_CURVE('',#691,#692,#411,.T.);
#834=EDGE_CURVE('',#692,#693,#608,.T.);
#835=EDGE_CURVE('',#693,#690,#412,.T.);
#836=EDGE_CURVE('',#694,#693,#413,.T.);
#837=EDGE_CURVE('',#695,#694,#414,.T.);
#838=EDGE_CURVE('',#690,#695,#415,.T.);
#839=EDGE_CURVE('',#696,#692,#416,.T.);
#840=EDGE_CURVE('',#696,#697,#417,.T.);
#841=EDGE_CURVE('',#698,#697,#418,.T.);
#842=EDGE_CURVE('',#694,#698,#609,.T.);
#843=EDGE_CURVE('',#698,#699,#419,.T.);
#844=EDGE_CURVE('',#699,#695,#610,.T.);
#845=EDGE_CURVE('',#700,#691,#420,.T.);
#846=EDGE_CURVE('',#700,#701,#421,.T.);
#847=EDGE_CURVE('',#701,#702,#422,.T.);
#848=EDGE_CURVE('',#696,#702,#423,.T.);
#849=EDGE_CURVE('',#703,#704,#611,.T.);
#850=EDGE_CURVE('',#705,#703,#424,.T.);
#851=EDGE_CURVE('',#706,#705,#612,.T.);
#852=EDGE_CURVE('',#704,#706,#425,.T.);
#853=EDGE_CURVE('',#697,#705,#426,.T.);
#854=EDGE_CURVE('',#702,#707,#613,.T.);
#855=EDGE_CURVE('',#707,#706,#427,.T.);
#856=EDGE_CURVE('',#707,#708,#428,.T.);
#857=EDGE_CURVE('',#704,#708,#429,.T.);
#858=EDGE_CURVE('',#708,#701,#614,.T.);
#859=EDGE_CURVE('',#699,#709,#430,.T.);
#860=EDGE_CURVE('',#709,#700,#431,.T.);
#861=EDGE_CURVE('',#709,#703,#432,.T.);
#862=EDGE_CURVE('',#710,#710,#615,.T.);
#863=EDGE_CURVE('',#711,#711,#616,.T.);
#864=EDGE_CURVE('',#711,#712,#617,.T.);
#865=EDGE_CURVE('',#712,#712,#618,.T.);
#866=EDGE_CURVE('',#713,#714,#433,.T.);
#867=EDGE_CURVE('',#714,#715,#434,.T.);
#868=EDGE_CURVE('',#715,#716,#435,.T.);
#869=EDGE_CURVE('',#716,#717,#436,.T.);
#870=EDGE_CURVE('',#717,#718,#437,.T.);
#871=EDGE_CURVE('',#718,#713,#438,.T.);
#872=EDGE_CURVE('',#719,#719,#619,.T.);
#873=EDGE_CURVE('',#719,#711,#439,.T.);
#874=EDGE_CURVE('',#720,#721,#440,.T.);
#875=EDGE_CURVE('',#722,#720,#441,.T.);
#876=EDGE_CURVE('',#722,#721,#442,.T.);
#877=EDGE_CURVE('',#723,#722,#443,.T.);
#878=EDGE_CURVE('',#723,#721,#444,.T.);
#879=EDGE_CURVE('',#724,#723,#445,.T.);
#880=EDGE_CURVE('',#724,#721,#446,.T.);
#881=EDGE_CURVE('',#725,#724,#447,.T.);
#882=EDGE_CURVE('',#725,#721,#448,.T.);
#883=EDGE_CURVE('',#726,#725,#449,.T.);
#884=EDGE_CURVE('',#726,#721,#450,.T.);
#885=EDGE_CURVE('',#720,#726,#451,.T.);
#886=EDGE_CURVE('',#713,#722,#452,.T.);
#887=EDGE_CURVE('',#714,#720,#453,.T.);
#888=EDGE_CURVE('',#718,#723,#454,.T.);
#889=EDGE_CURVE('',#717,#724,#455,.T.);
#890=EDGE_CURVE('',#716,#725,#456,.T.);
#891=EDGE_CURVE('',#715,#726,#457,.T.);
#892=EDGE_CURVE('',#710,#727,#458,.T.);
#893=EDGE_CURVE('',#727,#727,#620,.F.);
#894=ORIENTED_EDGE('',*,*,#728,.F.);
#895=ORIENTED_EDGE('',*,*,#729,.T.);
#896=ORIENTED_EDGE('',*,*,#730,.T.);
#897=ORIENTED_EDGE('',*,*,#729,.F.);
#898=ORIENTED_EDGE('',*,*,#728,.T.);
#899=ORIENTED_EDGE('',*,*,#730,.F.);
#900=ORIENTED_EDGE('',*,*,#731,.T.);
#901=ORIENTED_EDGE('',*,*,#732,.T.);
#902=ORIENTED_EDGE('',*,*,#733,.T.);
#903=ORIENTED_EDGE('',*,*,#734,.T.);
#904=ORIENTED_EDGE('',*,*,#733,.F.);
#905=ORIENTED_EDGE('',*,*,#735,.F.);
#906=ORIENTED_EDGE('',*,*,#736,.F.);
#907=ORIENTED_EDGE('',*,*,#737,.F.);
#908=ORIENTED_EDGE('',*,*,#738,.T.);
#909=ORIENTED_EDGE('',*,*,#739,.T.);
#910=ORIENTED_EDGE('',*,*,#732,.F.);
#911=ORIENTED_EDGE('',*,*,#740,.T.);
#912=ORIENTED_EDGE('',*,*,#741,.F.);
#913=ORIENTED_EDGE('',*,*,#735,.T.);
#914=ORIENTED_EDGE('',*,*,#736,.T.);
#915=ORIENTED_EDGE('',*,*,#741,.T.);
#916=ORIENTED_EDGE('',*,*,#742,.T.);
#917=ORIENTED_EDGE('',*,*,#743,.T.);
#918=ORIENTED_EDGE('',*,*,#744,.T.);
#919=ORIENTED_EDGE('',*,*,#745,.T.);
#920=ORIENTED_EDGE('',*,*,#746,.T.);
#921=ORIENTED_EDGE('',*,*,#747,.T.);
#922=ORIENTED_EDGE('',*,*,#747,.F.);
#923=ORIENTED_EDGE('',*,*,#748,.F.);
#924=ORIENTED_EDGE('',*,*,#749,.F.);
#925=ORIENTED_EDGE('',*,*,#750,.F.);
#926=ORIENTED_EDGE('',*,*,#746,.F.);
#927=ORIENTED_EDGE('',*,*,#751,.F.);
#928=ORIENTED_EDGE('',*,*,#752,.F.);
#929=ORIENTED_EDGE('',*,*,#753,.F.);
#930=ORIENTED_EDGE('',*,*,#754,.F.);
#931=ORIENTED_EDGE('',*,*,#748,.T.);
#932=ORIENTED_EDGE('',*,*,#755,.T.);
#933=ORIENTED_EDGE('',*,*,#749,.T.);
#934=ORIENTED_EDGE('',*,*,#754,.T.);
#935=ORIENTED_EDGE('',*,*,#756,.T.);
#936=ORIENTED_EDGE('',*,*,#744,.F.);
#937=ORIENTED_EDGE('',*,*,#750,.T.);
#938=ORIENTED_EDGE('',*,*,#755,.F.);
#939=ORIENTED_EDGE('',*,*,#757,.T.);
#940=ORIENTED_EDGE('',*,*,#738,.F.);
#941=ORIENTED_EDGE('',*,*,#758,.T.);
#942=ORIENTED_EDGE('',*,*,#743,.F.);
#943=ORIENTED_EDGE('',*,*,#759,.F.);
#944=ORIENTED_EDGE('',*,*,#751,.T.);
#945=ORIENTED_EDGE('',*,*,#745,.F.);
#946=ORIENTED_EDGE('',*,*,#758,.F.);
#947=ORIENTED_EDGE('',*,*,#737,.T.);
#948=ORIENTED_EDGE('',*,*,#731,.F.);
#949=ORIENTED_EDGE('',*,*,#760,.F.);
#950=ORIENTED_EDGE('',*,*,#752,.T.);
#951=ORIENTED_EDGE('',*,*,#759,.T.);
#952=ORIENTED_EDGE('',*,*,#742,.F.);
#953=ORIENTED_EDGE('',*,*,#740,.F.);
#954=ORIENTED_EDGE('',*,*,#734,.F.);
#955=ORIENTED_EDGE('',*,*,#739,.F.);
#956=ORIENTED_EDGE('',*,*,#757,.F.);
#957=ORIENTED_EDGE('',*,*,#756,.F.);
#958=ORIENTED_EDGE('',*,*,#753,.T.);
#959=ORIENTED_EDGE('',*,*,#760,.T.);
#960=ORIENTED_EDGE('',*,*,#761,.F.);
#961=ORIENTED_EDGE('',*,*,#762,.T.);
#962=ORIENTED_EDGE('',*,*,#763,.T.);
#963=ORIENTED_EDGE('',*,*,#762,.F.);
#964=ORIENTED_EDGE('',*,*,#763,.F.);
#965=ORIENTED_EDGE('',*,*,#764,.T.);
#966=ORIENTED_EDGE('',*,*,#761,.T.);
#967=ORIENTED_EDGE('',*,*,#765,.T.);
#968=ORIENTED_EDGE('',*,*,#765,.F.);
#969=ORIENTED_EDGE('',*,*,#766,.T.);
#970=ORIENTED_EDGE('',*,*,#767,.T.);
#971=ORIENTED_EDGE('',*,*,#766,.F.);
#972=ORIENTED_EDGE('',*,*,#767,.F.);
#973=ORIENTED_EDGE('',*,*,#764,.F.);
#974=ORIENTED_EDGE('',*,*,#768,.T.);
#975=ORIENTED_EDGE('',*,*,#769,.F.);
#976=ORIENTED_EDGE('',*,*,#768,.F.);
#977=ORIENTED_EDGE('',*,*,#769,.T.);
#978=ORIENTED_EDGE('',*,*,#770,.T.);
#979=ORIENTED_EDGE('',*,*,#771,.T.);
#980=ORIENTED_EDGE('',*,*,#772,.F.);
#981=ORIENTED_EDGE('',*,*,#771,.F.);
#982=ORIENTED_EDGE('',*,*,#773,.T.);
#983=ORIENTED_EDGE('',*,*,#774,.T.);
#984=ORIENTED_EDGE('',*,*,#775,.F.);
#985=ORIENTED_EDGE('',*,*,#776,.F.);
#986=ORIENTED_EDGE('',*,*,#777,.T.);
#987=ORIENTED_EDGE('',*,*,#776,.T.);
#988=ORIENTED_EDGE('',*,*,#778,.F.);
#989=ORIENTED_EDGE('',*,*,#779,.F.);
#990=ORIENTED_EDGE('',*,*,#780,.T.);
#991=ORIENTED_EDGE('',*,*,#779,.T.);
#992=ORIENTED_EDGE('',*,*,#781,.F.);
#993=ORIENTED_EDGE('',*,*,#782,.F.);
#994=ORIENTED_EDGE('',*,*,#783,.T.);
#995=ORIENTED_EDGE('',*,*,#782,.T.);
#996=ORIENTED_EDGE('',*,*,#784,.F.);
#997=ORIENTED_EDGE('',*,*,#774,.F.);
#998=ORIENTED_EDGE('',*,*,#784,.T.);
#999=ORIENTED_EDGE('',*,*,#781,.T.);
#1000=ORIENTED_EDGE('',*,*,#778,.T.);
#1001=ORIENTED_EDGE('',*,*,#775,.T.);
#1002=ORIENTED_EDGE('',*,*,#772,.T.);
#1003=ORIENTED_EDGE('',*,*,#783,.F.);
#1004=ORIENTED_EDGE('',*,*,#773,.F.);
#1005=ORIENTED_EDGE('',*,*,#777,.F.);
#1006=ORIENTED_EDGE('',*,*,#780,.F.);
#1007=ORIENTED_EDGE('',*,*,#770,.F.);
#1008=ORIENTED_EDGE('',*,*,#785,.F.);
#1009=ORIENTED_EDGE('',*,*,#786,.T.);
#1010=ORIENTED_EDGE('',*,*,#787,.F.);
#1011=ORIENTED_EDGE('',*,*,#786,.F.);
#1012=ORIENTED_EDGE('',*,*,#788,.F.);
#1013=ORIENTED_EDGE('',*,*,#789,.T.);
#1014=ORIENTED_EDGE('',*,*,#790,.F.);
#1015=ORIENTED_EDGE('',*,*,#789,.F.);
#1016=ORIENTED_EDGE('',*,*,#791,.F.);
#1017=ORIENTED_EDGE('',*,*,#792,.T.);
#1018=ORIENTED_EDGE('',*,*,#793,.F.);
#1019=ORIENTED_EDGE('',*,*,#794,.F.);
#1020=ORIENTED_EDGE('',*,*,#795,.T.);
#1021=ORIENTED_EDGE('',*,*,#794,.T.);
#1022=ORIENTED_EDGE('',*,*,#796,.F.);
#1023=ORIENTED_EDGE('',*,*,#797,.F.);
#1024=ORIENTED_EDGE('',*,*,#798,.T.);
#1025=ORIENTED_EDGE('',*,*,#797,.T.);
#1026=ORIENTED_EDGE('',*,*,#799,.F.);
#1027=ORIENTED_EDGE('',*,*,#800,.F.);
#1028=ORIENTED_EDGE('',*,*,#801,.T.);
#1029=ORIENTED_EDGE('',*,*,#800,.T.);
#1030=ORIENTED_EDGE('',*,*,#802,.F.);
#1031=ORIENTED_EDGE('',*,*,#792,.F.);
#1032=ORIENTED_EDGE('',*,*,#802,.T.);
#1033=ORIENTED_EDGE('',*,*,#799,.T.);
#1034=ORIENTED_EDGE('',*,*,#796,.T.);
#1035=ORIENTED_EDGE('',*,*,#793,.T.);
#1036=ORIENTED_EDGE('',*,*,#785,.T.);
#1037=ORIENTED_EDGE('',*,*,#788,.T.);
#1038=ORIENTED_EDGE('',*,*,#801,.F.);
#1039=ORIENTED_EDGE('',*,*,#791,.T.);
#1040=ORIENTED_EDGE('',*,*,#795,.F.);
#1041=ORIENTED_EDGE('',*,*,#798,.F.);
#1042=ORIENTED_EDGE('',*,*,#787,.T.);
#1043=ORIENTED_EDGE('',*,*,#790,.T.);
#1044=ORIENTED_EDGE('',*,*,#803,.F.);
#1045=ORIENTED_EDGE('',*,*,#804,.T.);
#1046=ORIENTED_EDGE('',*,*,#805,.T.);
#1047=ORIENTED_EDGE('',*,*,#804,.F.);
#1048=ORIENTED_EDGE('',*,*,#803,.T.);
#1049=ORIENTED_EDGE('',*,*,#806,.T.);
#1050=ORIENTED_EDGE('',*,*,#807,.F.);
#1051=ORIENTED_EDGE('',*,*,#806,.F.);
#1052=ORIENTED_EDGE('',*,*,#807,.T.);
#1053=ORIENTED_EDGE('',*,*,#805,.F.);
#1054=ORIENTED_EDGE('',*,*,#808,.F.);
#1055=ORIENTED_EDGE('',*,*,#809,.T.);
#1056=ORIENTED_EDGE('',*,*,#810,.F.);
#1057=ORIENTED_EDGE('',*,*,#811,.T.);
#1058=ORIENTED_EDGE('',*,*,#812,.F.);
#1059=ORIENTED_EDGE('',*,*,#811,.F.);
#1060=ORIENTED_EDGE('',*,*,#813,.F.);
#1061=ORIENTED_EDGE('',*,*,#814,.F.);
#1062=ORIENTED_EDGE('',*,*,#809,.F.);
#1063=ORIENTED_EDGE('',*,*,#815,.F.);
#1064=ORIENTED_EDGE('',*,*,#816,.F.);
#1065=ORIENTED_EDGE('',*,*,#817,.T.);
#1066=ORIENTED_EDGE('',*,*,#813,.T.);
#1067=ORIENTED_EDGE('',*,*,#810,.T.);
#1068=ORIENTED_EDGE('',*,*,#814,.T.);
#1069=ORIENTED_EDGE('',*,*,#817,.F.);
#1070=ORIENTED_EDGE('',*,*,#818,.T.);
#1071=ORIENTED_EDGE('',*,*,#819,.T.);
#1072=ORIENTED_EDGE('',*,*,#820,.T.);
#1073=ORIENTED_EDGE('',*,*,#821,.T.);
#1074=ORIENTED_EDGE('',*,*,#816,.T.);
#1075=ORIENTED_EDGE('',*,*,#815,.T.);
#1076=ORIENTED_EDGE('',*,*,#822,.T.);
#1077=ORIENTED_EDGE('',*,*,#823,.F.);
#1078=ORIENTED_EDGE('',*,*,#822,.F.);
#1079=ORIENTED_EDGE('',*,*,#824,.F.);
#1080=ORIENTED_EDGE('',*,*,#825,.F.);
#1081=ORIENTED_EDGE('',*,*,#826,.F.);
#1082=ORIENTED_EDGE('',*,*,#819,.F.);
#1083=ORIENTED_EDGE('',*,*,#826,.T.);
#1084=ORIENTED_EDGE('',*,*,#827,.F.);
#1085=ORIENTED_EDGE('',*,*,#828,.F.);
#1086=ORIENTED_EDGE('',*,*,#820,.F.);
#1087=ORIENTED_EDGE('',*,*,#812,.T.);
#1088=ORIENTED_EDGE('',*,*,#828,.T.);
#1089=ORIENTED_EDGE('',*,*,#829,.F.);
#1090=ORIENTED_EDGE('',*,*,#830,.F.);
#1091=ORIENTED_EDGE('',*,*,#821,.F.);
#1092=ORIENTED_EDGE('',*,*,#830,.T.);
#1093=ORIENTED_EDGE('',*,*,#831,.F.);
#1094=ORIENTED_EDGE('',*,*,#824,.T.);
#1095=ORIENTED_EDGE('',*,*,#818,.F.);
#1096=ORIENTED_EDGE('',*,*,#808,.T.);
#1097=ORIENTED_EDGE('',*,*,#831,.T.);
#1098=ORIENTED_EDGE('',*,*,#829,.T.);
#1099=ORIENTED_EDGE('',*,*,#827,.T.);
#1100=ORIENTED_EDGE('',*,*,#825,.T.);
#1101=ORIENTED_EDGE('',*,*,#823,.T.);
#1102=ORIENTED_EDGE('',*,*,#832,.T.);
#1103=ORIENTED_EDGE('',*,*,#833,.T.);
#1104=ORIENTED_EDGE('',*,*,#834,.T.);
#1105=ORIENTED_EDGE('',*,*,#835,.T.);
#1106=ORIENTED_EDGE('',*,*,#835,.F.);
#1107=ORIENTED_EDGE('',*,*,#836,.F.);
#1108=ORIENTED_EDGE('',*,*,#837,.F.);
#1109=ORIENTED_EDGE('',*,*,#838,.F.);
#1110=ORIENTED_EDGE('',*,*,#834,.F.);
#1111=ORIENTED_EDGE('',*,*,#839,.F.);
#1112=ORIENTED_EDGE('',*,*,#840,.T.);
#1113=ORIENTED_EDGE('',*,*,#841,.F.);
#1114=ORIENTED_EDGE('',*,*,#842,.F.);
#1115=ORIENTED_EDGE('',*,*,#836,.T.);
#1116=ORIENTED_EDGE('',*,*,#842,.T.);
#1117=ORIENTED_EDGE('',*,*,#843,.T.);
#1118=ORIENTED_EDGE('',*,*,#844,.T.);
#1119=ORIENTED_EDGE('',*,*,#837,.T.);
#1120=ORIENTED_EDGE('',*,*,#833,.F.);
#1121=ORIENTED_EDGE('',*,*,#845,.F.);
#1122=ORIENTED_EDGE('',*,*,#846,.T.);
#1123=ORIENTED_EDGE('',*,*,#847,.T.);
#1124=ORIENTED_EDGE('',*,*,#848,.F.);
#1125=ORIENTED_EDGE('',*,*,#839,.T.);
#1126=ORIENTED_EDGE('',*,*,#849,.F.);
#1127=ORIENTED_EDGE('',*,*,#850,.F.);
#1128=ORIENTED_EDGE('',*,*,#851,.F.);
#1129=ORIENTED_EDGE('',*,*,#852,.F.);
#1130=ORIENTED_EDGE('',*,*,#851,.T.);
#1131=ORIENTED_EDGE('',*,*,#853,.F.);
#1132=ORIENTED_EDGE('',*,*,#840,.F.);
#1133=ORIENTED_EDGE('',*,*,#848,.T.);
#1134=ORIENTED_EDGE('',*,*,#854,.T.);
#1135=ORIENTED_EDGE('',*,*,#855,.T.);
#1136=ORIENTED_EDGE('',*,*,#852,.T.);
#1137=ORIENTED_EDGE('',*,*,#855,.F.);
#1138=ORIENTED_EDGE('',*,*,#856,.T.);
#1139=ORIENTED_EDGE('',*,*,#857,.F.);
#1140=ORIENTED_EDGE('',*,*,#854,.F.);
#1141=ORIENTED_EDGE('',*,*,#847,.F.);
#1142=ORIENTED_EDGE('',*,*,#858,.F.);
#1143=ORIENTED_EDGE('',*,*,#856,.F.);
#1144=ORIENTED_EDGE('',*,*,#832,.F.);
#1145=ORIENTED_EDGE('',*,*,#838,.T.);
#1146=ORIENTED_EDGE('',*,*,#844,.F.);
#1147=ORIENTED_EDGE('',*,*,#859,.T.);
#1148=ORIENTED_EDGE('',*,*,#860,.T.);
#1149=ORIENTED_EDGE('',*,*,#845,.T.);
#1150=ORIENTED_EDGE('',*,*,#849,.T.);
#1151=ORIENTED_EDGE('',*,*,#857,.T.);
#1152=ORIENTED_EDGE('',*,*,#858,.T.);
#1153=ORIENTED_EDGE('',*,*,#846,.F.);
#1154=ORIENTED_EDGE('',*,*,#860,.F.);
#1155=ORIENTED_EDGE('',*,*,#861,.T.);
#1156=ORIENTED_EDGE('',*,*,#843,.F.);
#1157=ORIENTED_EDGE('',*,*,#841,.T.);
#1158=ORIENTED_EDGE('',*,*,#853,.T.);
#1159=ORIENTED_EDGE('',*,*,#850,.T.);
#1160=ORIENTED_EDGE('',*,*,#861,.F.);
#1161=ORIENTED_EDGE('',*,*,#859,.F.);
#1162=ORIENTED_EDGE('',*,*,#862,.F.);
#1163=ORIENTED_EDGE('',*,*,#863,.T.);
#1164=ORIENTED_EDGE('',*,*,#864,.T.);
#1165=ORIENTED_EDGE('',*,*,#865,.T.);
#1166=ORIENTED_EDGE('',*,*,#864,.F.);
#1167=ORIENTED_EDGE('',*,*,#865,.F.);
#1168=ORIENTED_EDGE('',*,*,#866,.T.);
#1169=ORIENTED_EDGE('',*,*,#867,.T.);
#1170=ORIENTED_EDGE('',*,*,#868,.T.);
#1171=ORIENTED_EDGE('',*,*,#869,.T.);
#1172=ORIENTED_EDGE('',*,*,#870,.T.);
#1173=ORIENTED_EDGE('',*,*,#871,.T.);
#1174=ORIENTED_EDGE('',*,*,#872,.F.);
#1175=ORIENTED_EDGE('',*,*,#873,.T.);
#1176=ORIENTED_EDGE('',*,*,#863,.F.);
#1177=ORIENTED_EDGE('',*,*,#873,.F.);
#1178=ORIENTED_EDGE('',*,*,#874,.F.);
#1179=ORIENTED_EDGE('',*,*,#875,.F.);
#1180=ORIENTED_EDGE('',*,*,#876,.T.);
#1181=ORIENTED_EDGE('',*,*,#876,.F.);
#1182=ORIENTED_EDGE('',*,*,#877,.F.);
#1183=ORIENTED_EDGE('',*,*,#878,.T.);
#1184=ORIENTED_EDGE('',*,*,#878,.F.);
#1185=ORIENTED_EDGE('',*,*,#879,.F.);
#1186=ORIENTED_EDGE('',*,*,#880,.T.);
#1187=ORIENTED_EDGE('',*,*,#880,.F.);
#1188=ORIENTED_EDGE('',*,*,#881,.F.);
#1189=ORIENTED_EDGE('',*,*,#882,.T.);
#1190=ORIENTED_EDGE('',*,*,#882,.F.);
#1191=ORIENTED_EDGE('',*,*,#883,.F.);
#1192=ORIENTED_EDGE('',*,*,#884,.T.);
#1193=ORIENTED_EDGE('',*,*,#884,.F.);
#1194=ORIENTED_EDGE('',*,*,#885,.F.);
#1195=ORIENTED_EDGE('',*,*,#874,.T.);
#1196=ORIENTED_EDGE('',*,*,#866,.F.);
#1197=ORIENTED_EDGE('',*,*,#886,.T.);
#1198=ORIENTED_EDGE('',*,*,#875,.T.);
#1199=ORIENTED_EDGE('',*,*,#887,.F.);
#1200=ORIENTED_EDGE('',*,*,#871,.F.);
#1201=ORIENTED_EDGE('',*,*,#888,.T.);
#1202=ORIENTED_EDGE('',*,*,#877,.T.);
#1203=ORIENTED_EDGE('',*,*,#886,.F.);
#1204=ORIENTED_EDGE('',*,*,#870,.F.);
#1205=ORIENTED_EDGE('',*,*,#889,.T.);
#1206=ORIENTED_EDGE('',*,*,#879,.T.);
#1207=ORIENTED_EDGE('',*,*,#888,.F.);
#1208=ORIENTED_EDGE('',*,*,#869,.F.);
#1209=ORIENTED_EDGE('',*,*,#890,.T.);
#1210=ORIENTED_EDGE('',*,*,#881,.T.);
#1211=ORIENTED_EDGE('',*,*,#889,.F.);
#1212=ORIENTED_EDGE('',*,*,#868,.F.);
#1213=ORIENTED_EDGE('',*,*,#891,.T.);
#1214=ORIENTED_EDGE('',*,*,#883,.T.);
#1215=ORIENTED_EDGE('',*,*,#890,.F.);
#1216=ORIENTED_EDGE('',*,*,#867,.F.);
#1217=ORIENTED_EDGE('',*,*,#887,.T.);
#1218=ORIENTED_EDGE('',*,*,#885,.T.);
#1219=ORIENTED_EDGE('',*,*,#891,.F.);
#1220=ORIENTED_EDGE('',*,*,#862,.T.);
#1221=ORIENTED_EDGE('',*,*,#892,.T.);
#1222=ORIENTED_EDGE('',*,*,#893,.T.);
#1223=ORIENTED_EDGE('',*,*,#892,.F.);
#1224=ORIENTED_EDGE('',*,*,#872,.T.);
#1225=ORIENTED_EDGE('',*,*,#893,.F.);
#1226=CYLINDRICAL_SURFACE('',#1438,8.);
#1227=CYLINDRICAL_SURFACE('',#1444,3.);
#1228=CYLINDRICAL_SURFACE('',#1450,3.);
#1229=CYLINDRICAL_SURFACE('',#1452,3.);
#1230=CYLINDRICAL_SURFACE('',#1458,3.);
#1231=CYLINDRICAL_SURFACE('',#1465,10.);
#1232=CYLINDRICAL_SURFACE('',#1472,20.);
#1233=CYLINDRICAL_SURFACE('',#1475,127.);
#1234=CYLINDRICAL_SURFACE('',#1479,152.4);
#1235=CYLINDRICAL_SURFACE('',#1489,10.);
#1236=CYLINDRICAL_SURFACE('',#1492,10.);
#1237=CYLINDRICAL_SURFACE('',#1502,152.4);
#1238=CYLINDRICAL_SURFACE('',#1510,9.89525);
#1239=CYLINDRICAL_SURFACE('',#1513,8.);
#1240=CYLINDRICAL_SURFACE('',#1516,8.);
#1241=CYLINDRICAL_SURFACE('',#1524,2.);
#1242=CYLINDRICAL_SURFACE('',#1530,2.);
#1243=CYLINDRICAL_SURFACE('',#1533,3.);
#1244=CYLINDRICAL_SURFACE('',#1539,3.);
#1245=CYLINDRICAL_SURFACE('',#1552,15.);
#1246=CYLINDRICAL_SURFACE('',#1566,9.89525);
#1247=ADVANCED_FACE('',(#165),#1226,.T.);
#1248=ADVANCED_FACE('',(#166),#108,.T.);
#1249=ADVANCED_FACE('',(#167),#109,.F.);
#1250=ADVANCED_FACE('',(#168),#1227,.T.);
#1251=ADVANCED_FACE('',(#169),#110,.T.);
#1252=ADVANCED_FACE('',(#170),#111,.T.);
#1253=ADVANCED_FACE('',(#171),#1228,.T.);
#1254=ADVANCED_FACE('',(#172),#1229,.T.);
#1255=ADVANCED_FACE('',(#173),#112,.T.);
#1256=ADVANCED_FACE('',(#174),#113,.F.);
#1257=ADVANCED_FACE('',(#175),#1230,.T.);
#1258=ADVANCED_FACE('',(#176),#114,.T.);
#1259=ADVANCED_FACE('',(#177),#115,.T.);
#1260=ADVANCED_FACE('',(#178),#116,.T.);
#1261=ADVANCED_FACE('',(#179),#117,.T.);
#1262=ADVANCED_FACE('',(#180),#1231,.F.);
#1263=ADVANCED_FACE('',(#181),#118,.T.);
#1264=ADVANCED_FACE('',(#182,#57,#58),#119,.F.);
#1265=ADVANCED_FACE('',(#183),#1232,.F.);
#1266=ADVANCED_FACE('',(#184),#120,.T.);
#1267=ADVANCED_FACE('',(#185),#1233,.T.);
#1268=ADVANCED_FACE('',(#186),#121,.T.);
#1269=ADVANCED_FACE('',(#187),#1234,.F.);
#1270=ADVANCED_FACE('',(#188),#122,.T.);
#1271=ADVANCED_FACE('',(#189),#123,.T.);
#1272=ADVANCED_FACE('',(#190),#124,.T.);
#1273=ADVANCED_FACE('',(#191),#125,.T.);
#1274=ADVANCED_FACE('',(#192,#59),#126,.T.);
#1275=ADVANCED_FACE('',(#193,#60),#127,.F.);
#1276=ADVANCED_FACE('',(#194),#1235,.F.);
#1277=ADVANCED_FACE('',(#195),#1236,.F.);
#1278=ADVANCED_FACE('',(#196),#128,.T.);
#1279=ADVANCED_FACE('',(#197),#129,.T.);
#1280=ADVANCED_FACE('',(#198),#130,.T.);
#1281=ADVANCED_FACE('',(#199),#131,.T.);
#1282=ADVANCED_FACE('',(#200,#61,#62),#132,.T.);
#1283=ADVANCED_FACE('',(#201,#63,#64),#133,.F.);
#1284=ADVANCED_FACE('',(#202),#1237,.T.);
#1285=ADVANCED_FACE('',(#203),#56,.T.);
#1286=ADVANCED_FACE('',(#204),#134,.T.);
#1287=ADVANCED_FACE('',(#205),#135,.T.);
#1288=ADVANCED_FACE('',(#206,#65),#1238,.F.);
#1289=ADVANCED_FACE('',(#207),#1239,.F.);
#1290=ADVANCED_FACE('',(#208,#66),#136,.F.);
#1291=ADVANCED_FACE('',(#209),#1240,.F.);
#1292=ADVANCED_FACE('',(#210),#137,.T.);
#1293=ADVANCED_FACE('',(#211,#67),#138,.T.);
#1294=ADVANCED_FACE('',(#212),#139,.T.);
#1295=ADVANCED_FACE('',(#213,#68),#140,.T.);
#1296=ADVANCED_FACE('',(#214,#69),#141,.T.);
#1297=ADVANCED_FACE('',(#215),#1241,.T.);
#1298=ADVANCED_FACE('',(#216),#142,.F.);
#1299=ADVANCED_FACE('',(#217),#143,.F.);
#1300=ADVANCED_FACE('',(#218),#1242,.T.);
#1301=ADVANCED_FACE('',(#219),#144,.F.);
#1302=ADVANCED_FACE('',(#220),#1243,.T.);
#1303=ADVANCED_FACE('',(#221),#145,.F.);
#1304=ADVANCED_FACE('',(#222),#146,.F.);
#1305=ADVANCED_FACE('',(#223),#1244,.T.);
#1306=ADVANCED_FACE('',(#224),#147,.T.);
#1307=ADVANCED_FACE('',(#225),#148,.F.);
#1308=ADVANCED_FACE('',(#226),#149,.F.);
#1309=ADVANCED_FACE('',(#227),#150,.T.);
#1310=ADVANCED_FACE('',(#228),#51,.T.);
#1311=ADVANCED_FACE('',(#229,#70),#151,.T.);
#1312=ADVANCED_FACE('',(#230),#1245,.T.);
#1313=ADVANCED_FACE('',(#231),#152,.F.);
#1314=ADVANCED_FACE('',(#232),#153,.F.);
#1315=ADVANCED_FACE('',(#233),#154,.F.);
#1316=ADVANCED_FACE('',(#234),#155,.F.);
#1317=ADVANCED_FACE('',(#235),#156,.F.);
#1318=ADVANCED_FACE('',(#236),#157,.F.);
#1319=ADVANCED_FACE('',(#237),#158,.F.);
#1320=ADVANCED_FACE('',(#238),#159,.F.);
#1321=ADVANCED_FACE('',(#239),#160,.F.);
#1322=ADVANCED_FACE('',(#240),#161,.F.);
#1323=ADVANCED_FACE('',(#241),#162,.F.);
#1324=ADVANCED_FACE('',(#242),#163,.F.);
#1325=ADVANCED_FACE('',(#243),#1246,.T.);
#1326=ADVANCED_FACE('',(#244,#71),#164,.T.);
#1327=CLOSED_SHELL('',(#1247,#1248,#1249));
#1328=CLOSED_SHELL('',(#1250,#1251,#1252,#1253,#1254,#1255,#1256,#1257,
#1258,#1259,#1260,#1261));
#1329=CLOSED_SHELL('',(#1262,#1263,#1264,#1265,#1266,#1267,#1268));
#1330=CLOSED_SHELL('',(#1269,#1270,#1271,#1272,#1273,#1274,#1275));
#1331=CLOSED_SHELL('',(#1276,#1277,#1278,#1279,#1280,#1281,#1282,#1283));
#1332=CLOSED_SHELL('',(#1284,#1285,#1286,#1287));
#1333=CLOSED_SHELL('',(#1288,#1289,#1290,#1291,#1292,#1293,#1294,#1295,
#1296));
#1334=CLOSED_SHELL('',(#1297,#1298,#1299,#1300,#1301,#1302,#1303,#1304,
#1305,#1306,#1307,#1308));
#1335=CLOSED_SHELL('',(#1309,#1310,#1311,#1312,#1313,#1314,#1315,#1316,
#1317,#1318,#1319,#1320,#1321,#1322,#1323,#1324,#1325,#1326));
#1336=DERIVED_UNIT_ELEMENT(#1354,1.);
#1337=DERIVED_UNIT_ELEMENT(#2464,-3.);
#1338=DERIVED_UNIT_ELEMENT(#1354,1.);
#1339=DERIVED_UNIT_ELEMENT(#2464,-3.);
#1340=DERIVED_UNIT_ELEMENT(#1354,1.);
#1341=DERIVED_UNIT_ELEMENT(#2464,-3.);
#1342=DERIVED_UNIT_ELEMENT(#1354,1.);
#1343=DERIVED_UNIT_ELEMENT(#2464,-3.);
#1344=DERIVED_UNIT_ELEMENT(#1354,1.);
#1345=DERIVED_UNIT_ELEMENT(#2464,-3.);
#1346=DERIVED_UNIT_ELEMENT(#1354,1.);
#1347=DERIVED_UNIT_ELEMENT(#2464,-3.);
#1348=DERIVED_UNIT_ELEMENT(#1354,1.);
#1349=DERIVED_UNIT_ELEMENT(#2464,-3.);
#1350=DERIVED_UNIT_ELEMENT(#1354,1.);
#1351=DERIVED_UNIT_ELEMENT(#2464,-3.);
#1352=DERIVED_UNIT_ELEMENT(#1354,1.);
#1353=DERIVED_UNIT_ELEMENT(#2464,-3.);
#1354=(
MASS_UNIT()
NAMED_UNIT(*)
SI_UNIT(.KILO.,.GRAM.)
);
#1355=DERIVED_UNIT((#1336,#1337));
#1356=DERIVED_UNIT((#1338,#1339));
#1357=DERIVED_UNIT((#1340,#1341));
#1358=DERIVED_UNIT((#1342,#1343));
#1359=DERIVED_UNIT((#1344,#1345));
#1360=DERIVED_UNIT((#1346,#1347));
#1361=DERIVED_UNIT((#1348,#1349));
#1362=DERIVED_UNIT((#1350,#1351));
#1363=DERIVED_UNIT((#1352,#1353));
#1364=MEASURE_REPRESENTATION_ITEM('density measure',
POSITIVE_RATIO_MEASURE(7850.),#1355);
#1365=MEASURE_REPRESENTATION_ITEM('density measure',
POSITIVE_RATIO_MEASURE(7850.),#1356);
#1366=MEASURE_REPRESENTATION_ITEM('density measure',
POSITIVE_RATIO_MEASURE(7850.),#1357);
#1367=MEASURE_REPRESENTATION_ITEM('density measure',
POSITIVE_RATIO_MEASURE(7850.),#1358);
#1368=MEASURE_REPRESENTATION_ITEM('density measure',
POSITIVE_RATIO_MEASURE(7850.),#1359);
#1369=MEASURE_REPRESENTATION_ITEM('density measure',
POSITIVE_RATIO_MEASURE(7850.),#1360);
#1370=MEASURE_REPRESENTATION_ITEM('density measure',
POSITIVE_RATIO_MEASURE(7850.),#1361);
#1371=MEASURE_REPRESENTATION_ITEM('density measure',
POSITIVE_RATIO_MEASURE(7850.),#1362);
#1372=MEASURE_REPRESENTATION_ITEM('density measure',
POSITIVE_RATIO_MEASURE(7750.),#1363);
#1373=PROPERTY_DEFINITION_REPRESENTATION(#1418,#1391);
#1374=PROPERTY_DEFINITION_REPRESENTATION(#1419,#1392);
#1375=PROPERTY_DEFINITION_REPRESENTATION(#1420,#1393);
#1376=PROPERTY_DEFINITION_REPRESENTATION(#1421,#1394);
#1377=PROPERTY_DEFINITION_REPRESENTATION(#1422,#1395);
#1378=PROPERTY_DEFINITION_REPRESENTATION(#1423,#1396);
#1379=PROPERTY_DEFINITION_REPRESENTATION(#1424,#1397);
#1380=PROPERTY_DEFINITION_REPRESENTATION(#1425,#1398);
#1381=PROPERTY_DEFINITION_REPRESENTATION(#1426,#1399);
#1382=PROPERTY_DEFINITION_REPRESENTATION(#1427,#1400);
#1383=PROPERTY_DEFINITION_REPRESENTATION(#1428,#1401);
#1384=PROPERTY_DEFINITION_REPRESENTATION(#1429,#1402);
#1385=PROPERTY_DEFINITION_REPRESENTATION(#1430,#1403);
#1386=PROPERTY_DEFINITION_REPRESENTATION(#1431,#1404);
#1387=PROPERTY_DEFINITION_REPRESENTATION(#1432,#1405);
#1388=PROPERTY_DEFINITION_REPRESENTATION(#1433,#1406);
#1389=PROPERTY_DEFINITION_REPRESENTATION(#1434,#1407);
#1390=PROPERTY_DEFINITION_REPRESENTATION(#1435,#1408);
#1391=REPRESENTATION('material name',(#1409),#2453);
#1392=REPRESENTATION('density',(#1364),#2453);
#1393=REPRESENTATION('material name',(#1410),#2454);
#1394=REPRESENTATION('density',(#1365),#2454);
#1395=REPRESENTATION('material name',(#1411),#2455);
#1396=REPRESENTATION('density',(#1366),#2455);
#1397=REPRESENTATION('material name',(#1412),#2456);
#1398=REPRESENTATION('density',(#1367),#2456);
#1399=REPRESENTATION('material name',(#1413),#2457);
#1400=REPRESENTATION('density',(#1368),#2457);
#1401=REPRESENTATION('material name',(#1414),#2458);
#1402=REPRESENTATION('density',(#1369),#2458);
#1403=REPRESENTATION('material name',(#1415),#2459);
#1404=REPRESENTATION('density',(#1370),#2459);
#1405=REPRESENTATION('material name',(#1416),#2460);
#1406=REPRESENTATION('density',(#1371),#2460);
#1407=REPRESENTATION('material name',(#1417),#2461);
#1408=REPRESENTATION('density',(#1372),#2461);
#1409=DESCRIPTIVE_REPRESENTATION_ITEM('Steel','Steel');
#1410=DESCRIPTIVE_REPRESENTATION_ITEM('Steel','Steel');
#1411=DESCRIPTIVE_REPRESENTATION_ITEM('Steel','Steel');
#1412=DESCRIPTIVE_REPRESENTATION_ITEM('Steel','Steel');
#1413=DESCRIPTIVE_REPRESENTATION_ITEM('Steel','Steel');
#1414=DESCRIPTIVE_REPRESENTATION_ITEM('Steel','Steel');
#1415=DESCRIPTIVE_REPRESENTATION_ITEM('Steel','Steel');
#1416=DESCRIPTIVE_REPRESENTATION_ITEM('Steel','Steel');
#1417=DESCRIPTIVE_REPRESENTATION_ITEM('Steel Grade 2, Plain',
'Steel Grade 2, Plain');
#1418=PROPERTY_DEFINITION('material property','material name',#2509);
#1419=PROPERTY_DEFINITION('material property','density of part',#2509);
#1420=PROPERTY_DEFINITION('material property','material name',#2510);
#1421=PROPERTY_DEFINITION('material property','density of part',#2510);
#1422=PROPERTY_DEFINITION('material property','material name',#2511);
#1423=PROPERTY_DEFINITION('material property','density of part',#2511);
#1424=PROPERTY_DEFINITION('material property','material name',#2512);
#1425=PROPERTY_DEFINITION('material property','density of part',#2512);
#1426=PROPERTY_DEFINITION('material property','material name',#2513);
#1427=PROPERTY_DEFINITION('material property','density of part',#2513);
#1428=PROPERTY_DEFINITION('material property','material name',#2514);
#1429=PROPERTY_DEFINITION('material property','density of part',#2514);
#1430=PROPERTY_DEFINITION('material property','material name',#2515);
#1431=PROPERTY_DEFINITION('material property','density of part',#2515);
#1432=PROPERTY_DEFINITION('material property','material name',#2516);
#1433=PROPERTY_DEFINITION('material property','density of part',#2516);
#1434=PROPERTY_DEFINITION('material property','material name',#2517);
#1435=PROPERTY_DEFINITION('material property','density of part',#2517);
#1436=AXIS2_PLACEMENT_3D('',#1984,#1579,#1580);
#1437=AXIS2_PLACEMENT_3D('',#1985,#1581,#1582);
#1438=AXIS2_PLACEMENT_3D('',#1986,#1583,#1584);
#1439=AXIS2_PLACEMENT_3D('',#1988,#1585,#1586);
#1440=AXIS2_PLACEMENT_3D('',#1991,#1588,#1589);
#1441=AXIS2_PLACEMENT_3D('',#1992,#1590,#1591);
#1442=AXIS2_PLACEMENT_3D('',#1993,#1592,#1593);
#1443=AXIS2_PLACEMENT_3D('',#1994,#1594,#1595);
#1444=AXIS2_PLACEMENT_3D('',#1995,#1596,#1597);
#1445=AXIS2_PLACEMENT_3D('',#1998,#1598,#1599);
#1446=AXIS2_PLACEMENT_3D('',#2002,#1601,#1602);
#1447=AXIS2_PLACEMENT_3D('',#2004,#1604,#1605);
#1448=AXIS2_PLACEMENT_3D('',#2008,#1607,#1608);
#1449=AXIS2_PLACEMENT_3D('',#2014,#1612,#1613);
#1450=AXIS2_PLACEMENT_3D('',#2018,#1616,#1617);
#1451=AXIS2_PLACEMENT_3D('',#2020,#1618,#1619);
#1452=AXIS2_PLACEMENT_3D('',#2022,#1621,#1622);
#1453=AXIS2_PLACEMENT_3D('',#2025,#1623,#1624);
#1454=AXIS2_PLACEMENT_3D('',#2029,#1626,#1627);
#1455=AXIS2_PLACEMENT_3D('',#2031,#1629,#1630);
#1456=AXIS2_PLACEMENT_3D('',#2037,#1634,#1635);
#1457=AXIS2_PLACEMENT_3D('',#2044,#1639,#1640);
#1458=AXIS2_PLACEMENT_3D('',#2045,#1641,#1642);
#1459=AXIS2_PLACEMENT_3D('',#2047,#1643,#1644);
#1460=AXIS2_PLACEMENT_3D('',#2049,#1646,#1647);
#1461=AXIS2_PLACEMENT_3D('',#2052,#1650,#1651);
#1462=AXIS2_PLACEMENT_3D('',#2054,#1653,#1654);
#1463=AXIS2_PLACEMENT_3D('',#2056,#1656,#1657);
#1464=AXIS2_PLACEMENT_3D('',#2057,#1658,#1659);
#1465=AXIS2_PLACEMENT_3D('',#2058,#1660,#1661);
#1466=AXIS2_PLACEMENT_3D('',#2060,#1662,#1663);
#1467=AXIS2_PLACEMENT_3D('',#2063,#1665,#1666);
#1468=AXIS2_PLACEMENT_3D('',#2064,#1667,#1668);
#1469=AXIS2_PLACEMENT_3D('',#2065,#1669,#1670);
#1470=AXIS2_PLACEMENT_3D('',#2067,#1671,#1672);
#1471=AXIS2_PLACEMENT_3D('',#2069,#1673,#1674);
#1472=AXIS2_PLACEMENT_3D('',#2070,#1675,#1676);
#1473=AXIS2_PLACEMENT_3D('',#2073,#1678,#1679);
#1474=AXIS2_PLACEMENT_3D('',#2074,#1680,#1681);
#1475=AXIS2_PLACEMENT_3D('',#2075,#1682,#1683);
#1476=AXIS2_PLACEMENT_3D('',#2078,#1685,#1686);
#1477=AXIS2_PLACEMENT_3D('',#2079,#1687,#1688);
#1478=AXIS2_PLACEMENT_3D('',#2080,#1689,#1690);
#1479=AXIS2_PLACEMENT_3D('',#2081,#1691,#1692);
#1480=AXIS2_PLACEMENT_3D('',#2083,#1693,#1694);
#1481=AXIS2_PLACEMENT_3D('',#2086,#1696,#1697);
#1482=AXIS2_PLACEMENT_3D('',#2087,#1698,#1699);
#1483=AXIS2_PLACEMENT_3D('',#2096,#1704,#1705);
#1484=AXIS2_PLACEMENT_3D('',#2102,#1709,#1710);
#1485=AXIS2_PLACEMENT_3D('',#2108,#1714,#1715);
#1486=AXIS2_PLACEMENT_3D('',#2111,#1718,#1719);
#1487=AXIS2_PLACEMENT_3D('',#2112,#1720,#1721);
#1488=AXIS2_PLACEMENT_3D('',#2113,#1722,#1723);
#1489=AXIS2_PLACEMENT_3D('',#2114,#1724,#1725);
#1490=AXIS2_PLACEMENT_3D('',#2116,#1726,#1727);
#1491=AXIS2_PLACEMENT_3D('',#2119,#1729,#1730);
#1492=AXIS2_PLACEMENT_3D('',#2120,#1731,#1732);
#1493=AXIS2_PLACEMENT_3D('',#2122,#1733,#1734);
#1494=AXIS2_PLACEMENT_3D('',#2125,#1736,#1737);
#1495=AXIS2_PLACEMENT_3D('',#2126,#1738,#1739);
#1496=AXIS2_PLACEMENT_3D('',#2135,#1744,#1745);
#1497=AXIS2_PLACEMENT_3D('',#2141,#1749,#1750);
#1498=AXIS2_PLACEMENT_3D('',#2147,#1754,#1755);
#1499=AXIS2_PLACEMENT_3D('',#2150,#1758,#1759);
#1500=AXIS2_PLACEMENT_3D('',#2151,#1760,#1761);
#1501=AXIS2_PLACEMENT_3D('',#2152,#1762,#1763);
#1502=AXIS2_PLACEMENT_3D('',#2153,#1764,#1765);
#1503=AXIS2_PLACEMENT_3D('',#2155,#1766,#1767);
#1504=AXIS2_PLACEMENT_3D('',#2158,#1769,#1770);
#1505=AXIS2_PLACEMENT_3D('',#2159,#1771,#1772);
#1506=AXIS2_PLACEMENT_3D('',#2162,#1774,#1775);
#1507=AXIS2_PLACEMENT_3D('',#2163,#1776,#1777);
#1508=AXIS2_PLACEMENT_3D('',#2164,#1778,#1779);
#1509=AXIS2_PLACEMENT_3D('',#2165,#1780,#1781);
#1510=AXIS2_PLACEMENT_3D('',#2166,#1782,#1783);
#1511=AXIS2_PLACEMENT_3D('',#2168,#1784,#1785);
#1512=AXIS2_PLACEMENT_3D('',#2196,#1788,#1789);
#1513=AXIS2_PLACEMENT_3D('',#2265,#1790,#1791);
#1514=AXIS2_PLACEMENT_3D('',#2267,#1792,#1793);
#1515=AXIS2_PLACEMENT_3D('',#2269,#1795,#1796);
#1516=AXIS2_PLACEMENT_3D('',#2278,#1801,#1802);
#1517=AXIS2_PLACEMENT_3D('',#2281,#1804,#1805);
#1518=AXIS2_PLACEMENT_3D('',#2282,#1806,#1807);
#1519=AXIS2_PLACEMENT_3D('',#2288,#1811,#1812);
#1520=AXIS2_PLACEMENT_3D('',#2292,#1815,#1816);
#1521=AXIS2_PLACEMENT_3D('',#2296,#1819,#1820);
#1522=AXIS2_PLACEMENT_3D('',#2298,#1822,#1823);
#1523=AXIS2_PLACEMENT_3D('',#2299,#1824,#1825);
#1524=AXIS2_PLACEMENT_3D('',#2300,#1826,#1827);
#1525=AXIS2_PLACEMENT_3D('',#2303,#1828,#1829);
#1526=AXIS2_PLACEMENT_3D('',#2307,#1831,#1832);
#1527=AXIS2_PLACEMENT_3D('',#2309,#1834,#1835);
#1528=AXIS2_PLACEMENT_3D('',#2315,#1839,#1840);
#1529=AXIS2_PLACEMENT_3D('',#2322,#1844,#1845);
#1530=AXIS2_PLACEMENT_3D('',#2323,#1846,#1847);
#1531=AXIS2_PLACEMENT_3D('',#2326,#1849,#1850);
#1532=AXIS2_PLACEMENT_3D('',#2327,#1851,#1852);
#1533=AXIS2_PLACEMENT_3D('',#2335,#1857,#1858);
#1534=AXIS2_PLACEMENT_3D('',#2338,#1859,#1860);
#1535=AXIS2_PLACEMENT_3D('',#2342,#1862,#1863);
#1536=AXIS2_PLACEMENT_3D('',#2344,#1865,#1866);
#1537=AXIS2_PLACEMENT_3D('',#2347,#1868,#1869);
#1538=AXIS2_PLACEMENT_3D('',#2349,#1871,#1872);
#1539=AXIS2_PLACEMENT_3D('',#2353,#1875,#1876);
#1540=AXIS2_PLACEMENT_3D('',#2354,#1877,#1878);
#1541=AXIS2_PLACEMENT_3D('',#2355,#1879,#1880);
#1542=AXIS2_PLACEMENT_3D('',#2359,#1883,#1884);
#1543=AXIS2_PLACEMENT_3D('',#2361,#1886,#1887);
#1544=AXIS2_PLACEMENT_3D('',#2362,#1888,#1889);
#1545=AXIS2_PLACEMENT_3D('',#2363,#1890,#1891);
#1546=AXIS2_PLACEMENT_3D('',#2365,#1892,#1893);
#1547=AXIS2_PLACEMENT_3D('',#2366,#1894,#1895);
#1548=AXIS2_PLACEMENT_3D('',#2368,#1896,#1897);
#1549=AXIS2_PLACEMENT_3D('',#2370,#1898,#1899);
#1550=AXIS2_PLACEMENT_3D('',#2371,#1900,#1901);
#1551=AXIS2_PLACEMENT_3D('',#2372,#1902,#1903);
#1552=AXIS2_PLACEMENT_3D('',#2385,#1910,#1911);
#1553=AXIS2_PLACEMENT_3D('',#2387,#1912,#1913);
#1554=AXIS2_PLACEMENT_3D('',#2389,#1915,#1916);
#1555=AXIS2_PLACEMENT_3D('',#2396,#1920,#1921);
#1556=AXIS2_PLACEMENT_3D('',#2400,#1924,#1925);
#1557=AXIS2_PLACEMENT_3D('',#2404,#1928,#1929);
#1558=AXIS2_PLACEMENT_3D('',#2408,#1932,#1933);
#1559=AXIS2_PLACEMENT_3D('',#2412,#1936,#1937);
#1560=AXIS2_PLACEMENT_3D('',#2414,#1939,#1940);
#1561=AXIS2_PLACEMENT_3D('',#2417,#1943,#1944);
#1562=AXIS2_PLACEMENT_3D('',#2419,#1946,#1947);
#1563=AXIS2_PLACEMENT_3D('',#2421,#1949,#1950);
#1564=AXIS2_PLACEMENT_3D('',#2423,#1952,#1953);
#1565=AXIS2_PLACEMENT_3D('',#2425,#1955,#1956);
#1566=AXIS2_PLACEMENT_3D('',#2426,#1957,#1958);
#1567=AXIS2_PLACEMENT_3D('',#2429,#1960,#1961);
#1568=AXIS2_PLACEMENT_3D('',#2430,#1962,#1963);
#1569=AXIS2_PLACEMENT_3D('',#2431,#1964,#1965);
#1570=AXIS2_PLACEMENT_3D('',#2432,#1966,#1967);
#1571=AXIS2_PLACEMENT_3D('',#2433,#1968,#1969);
#1572=AXIS2_PLACEMENT_3D('',#2434,#1970,#1971);
#1573=AXIS2_PLACEMENT_3D('',#2435,#1972,#1973);
#1574=AXIS2_PLACEMENT_3D('',#2436,#1974,#1975);
#1575=AXIS2_PLACEMENT_3D('',#2437,#1976,#1977);
#1576=AXIS2_PLACEMENT_3D('',#2438,#1978,#1979);
#1577=AXIS2_PLACEMENT_3D('',#2439,#1980,#1981);
#1578=AXIS2_PLACEMENT_3D('',#2440,#1982,#1983);
#1579=DIRECTION('axis',(0.,0.,1.));
#1580=DIRECTION('refdir',(1.,0.,0.));
#1581=DIRECTION('axis',(0.,0.,1.));
#1582=DIRECTION('refdir',(1.,0.,0.));
#1583=DIRECTION('center_axis',(1.,0.,0.));
#1584=DIRECTION('ref_axis',(0.,1.,0.));
#1585=DIRECTION('center_axis',(1.,0.,0.));
#1586=DIRECTION('ref_axis',(0.,1.,0.));
#1587=DIRECTION('',(-1.,0.,0.));
#1588=DIRECTION('center_axis',(1.,0.,0.));
#1589=DIRECTION('ref_axis',(0.,1.,0.));
#1590=DIRECTION('center_axis',(1.,0.,0.));
#1591=DIRECTION('ref_axis',(0.,0.,-1.));
#1592=DIRECTION('center_axis',(1.,0.,0.));
#1593=DIRECTION('ref_axis',(0.,0.,-1.));
#1594=DIRECTION('axis',(0.,0.,1.));
#1595=DIRECTION('refdir',(1.,0.,0.));
#1596=DIRECTION('center_axis',(0.,0.,-1.));
#1597=DIRECTION('ref_axis',(0.707106781186544,-0.707106781186551,0.));
#1598=DIRECTION('center_axis',(0.,0.,1.));
#1599=DIRECTION('ref_axis',(0.707106781186544,-0.707106781186551,0.));
#1600=DIRECTION('',(0.,0.,1.));
#1601=DIRECTION('center_axis',(0.,0.,-1.));
#1602=DIRECTION('ref_axis',(0.707106781186544,-0.707106781186551,0.));
#1603=DIRECTION('',(0.,0.,-1.));
#1604=DIRECTION('center_axis',(0.,0.,1.));
#1605=DIRECTION('ref_axis',(0.,-1.,0.));
#1606=DIRECTION('',(0.,-1.,0.));
#1607=DIRECTION('center_axis',(0.,0.,-1.));
#1608=DIRECTION('ref_axis',(0.707106781186544,0.707106781186551,0.));
#1609=DIRECTION('',(1.,0.,0.));
#1610=DIRECTION('',(0.,-1.,0.));
#1611=DIRECTION('',(1.,0.,0.));
#1612=DIRECTION('center_axis',(1.,0.,0.));
#1613=DIRECTION('ref_axis',(0.,0.,-1.));
#1614=DIRECTION('',(0.,1.,0.));
#1615=DIRECTION('',(0.,0.,-1.));
#1616=DIRECTION('center_axis',(0.,0.,1.));
#1617=DIRECTION('ref_axis',(0.707106781186544,0.707106781186551,0.));
#1618=DIRECTION('center_axis',(0.,0.,1.));
#1619=DIRECTION('ref_axis',(0.707106781186544,0.707106781186551,0.));
#1620=DIRECTION('',(0.,0.,1.));
#1621=DIRECTION('center_axis',(1.,0.,0.));
#1622=DIRECTION('ref_axis',(0.,0.707106781186547,0.707106781186547));
#1623=DIRECTION('center_axis',(-1.,0.,0.));
#1624=DIRECTION('ref_axis',(0.,0.707106781186547,0.707106781186547));
#1625=DIRECTION('',(-1.,0.,0.));
#1626=DIRECTION('center_axis',(1.,0.,0.));
#1627=DIRECTION('ref_axis',(0.,0.707106781186547,0.707106781186547));
#1628=DIRECTION('',(1.,0.,0.));
#1629=DIRECTION('center_axis',(0.,0.,1.));
#1630=DIRECTION('ref_axis',(0.,-1.,0.));
#1631=DIRECTION('',(0.,1.,0.));
#1632=DIRECTION('',(-1.,0.,0.));
#1633=DIRECTION('',(0.,-1.,0.));
#1634=DIRECTION('center_axis',(1.,0.,0.));
#1635=DIRECTION('ref_axis',(0.,1.,0.));
#1636=DIRECTION('',(0.,0.,1.));
#1637=DIRECTION('',(0.,1.,0.));
#1638=DIRECTION('',(0.,0.,-1.));
#1639=DIRECTION('center_axis',(1.,0.,0.));
#1640=DIRECTION('ref_axis',(0.,-0.707106781186547,0.707106781186547));
#1641=DIRECTION('center_axis',(1.,0.,0.));
#1642=DIRECTION('ref_axis',(0.,-0.707106781186547,0.707106781186547));
#1643=DIRECTION('center_axis',(-1.,0.,0.));
#1644=DIRECTION('ref_axis',(0.,-0.707106781186547,0.707106781186547));
#1645=DIRECTION('',(1.,0.,0.));
#1646=DIRECTION('center_axis',(1.,0.,0.));
#1647=DIRECTION('ref_axis',(0.,0.,-1.));
#1648=DIRECTION('',(0.,0.,-1.));
#1649=DIRECTION('',(0.,0.,1.));
#1650=DIRECTION('center_axis',(0.,1.,0.));
#1651=DIRECTION('ref_axis',(0.,0.,1.));
#1652=DIRECTION('',(1.,0.,0.));
#1653=DIRECTION('center_axis',(0.,0.,-1.));
#1654=DIRECTION('ref_axis',(0.,1.,0.));
#1655=DIRECTION('',(1.,0.,0.));
#1656=DIRECTION('center_axis',(0.,-1.,0.));
#1657=DIRECTION('ref_axis',(0.,0.,-1.));
#1658=DIRECTION('axis',(0.,0.,1.));
#1659=DIRECTION('refdir',(1.,0.,0.));
#1660=DIRECTION('center_axis',(0.,0.,-1.));
#1661=DIRECTION('ref_axis',(-1.,0.,0.));
#1662=DIRECTION('center_axis',(0.,0.,-1.));
#1663=DIRECTION('ref_axis',(-1.,0.,0.));
#1664=DIRECTION('',(0.,0.,-1.));
#1665=DIRECTION('center_axis',(0.,0.,-1.));
#1666=DIRECTION('ref_axis',(-1.,0.,0.));
#1667=DIRECTION('center_axis',(0.,0.,1.));
#1668=DIRECTION('ref_axis',(-1.,0.,0.));
#1669=DIRECTION('center_axis',(0.,0.,-1.));
#1670=DIRECTION('ref_axis',(-1.,0.,0.));
#1671=DIRECTION('center_axis',(0.,0.,1.));
#1672=DIRECTION('ref_axis',(-1.,0.,0.));
#1673=DIRECTION('center_axis',(0.,0.,-1.));
#1674=DIRECTION('ref_axis',(-1.,0.,0.));
#1675=DIRECTION('center_axis',(0.,0.,-1.));
#1676=DIRECTION('ref_axis',(-1.,0.,0.));
#1677=DIRECTION('',(0.,0.,-1.));
#1678=DIRECTION('center_axis',(0.,0.,-1.));
#1679=DIRECTION('ref_axis',(-1.,0.,0.));
#1680=DIRECTION('center_axis',(0.,0.,1.));
#1681=DIRECTION('ref_axis',(-1.,0.,0.));
#1682=DIRECTION('center_axis',(0.,0.,1.));
#1683=DIRECTION('ref_axis',(-1.,0.,0.));
#1684=DIRECTION('',(0.,0.,-1.));
#1685=DIRECTION('center_axis',(0.,0.,1.));
#1686=DIRECTION('ref_axis',(-1.,0.,0.));
#1687=DIRECTION('center_axis',(0.,0.,-1.));
#1688=DIRECTION('ref_axis',(-1.,0.,0.));
#1689=DIRECTION('axis',(0.,0.,1.));
#1690=DIRECTION('refdir',(1.,0.,0.));
#1691=DIRECTION('center_axis',(0.,0.,-1.));
#1692=DIRECTION('ref_axis',(-1.,0.,0.));
#1693=DIRECTION('center_axis',(0.,0.,1.));
#1694=DIRECTION('ref_axis',(-1.,0.,0.));
#1695=DIRECTION('',(0.,0.,-1.));
#1696=DIRECTION('center_axis',(0.,0.,1.));
#1697=DIRECTION('ref_axis',(-1.,0.,0.));
#1698=DIRECTION('center_axis',(0.,-1.,0.));
#1699=DIRECTION('ref_axis',(-1.,0.,0.));
#1700=DIRECTION('',(-1.,0.,0.));
#1701=DIRECTION('',(0.,0.,-1.));
#1702=DIRECTION('',(-1.,0.,0.));
#1703=DIRECTION('',(0.,0.,-1.));
#1704=DIRECTION('center_axis',(1.,0.,0.));
#1705=DIRECTION('ref_axis',(0.,-1.,0.));
#1706=DIRECTION('',(0.,-1.,0.));
#1707=DIRECTION('',(0.,-1.,0.));
#1708=DIRECTION('',(0.,0.,-1.));
#1709=DIRECTION('center_axis',(0.,1.,0.));
#1710=DIRECTION('ref_axis',(1.,0.,0.));
#1711=DIRECTION('',(1.,0.,0.));
#1712=DIRECTION('',(1.,0.,0.));
#1713=DIRECTION('',(0.,0.,-1.));
#1714=DIRECTION('center_axis',(-1.,0.,0.));
#1715=DIRECTION('ref_axis',(0.,1.,0.));
#1716=DIRECTION('',(0.,1.,0.));
#1717=DIRECTION('',(0.,1.,0.));
#1718=DIRECTION('center_axis',(0.,0.,-1.));
#1719=DIRECTION('ref_axis',(-1.,0.,0.));
#1720=DIRECTION('center_axis',(0.,0.,-1.));
#1721=DIRECTION('ref_axis',(-1.,0.,0.));
#1722=DIRECTION('axis',(0.,0.,1.));
#1723=DIRECTION('refdir',(1.,0.,0.));
#1724=DIRECTION('center_axis',(0.,0.,-1.));
#1725=DIRECTION('ref_axis',(-1.,0.,0.));
#1726=DIRECTION('center_axis',(0.,0.,-1.));
#1727=DIRECTION('ref_axis',(-1.,0.,0.));
#1728=DIRECTION('',(0.,0.,-1.));
#1729=DIRECTION('center_axis',(0.,0.,1.));
#1730=DIRECTION('ref_axis',(-1.,0.,0.));
#1731=DIRECTION('center_axis',(0.,0.,-1.));
#1732=DIRECTION('ref_axis',(-1.,0.,0.));
#1733=DIRECTION('center_axis',(0.,0.,-1.));
#1734=DIRECTION('ref_axis',(-1.,0.,0.));
#1735=DIRECTION('',(0.,0.,-1.));
#1736=DIRECTION('center_axis',(0.,0.,1.));
#1737=DIRECTION('ref_axis',(-1.,0.,0.));
#1738=DIRECTION('center_axis',(-0.261435213626798,-0.965221026022491,0.));
#1739=DIRECTION('ref_axis',(0.965221026022491,-0.261435213626798,0.));
#1740=DIRECTION('',(-0.965221026022491,0.261435213626798,0.));
#1741=DIRECTION('',(0.,0.,-1.));
#1742=DIRECTION('',(0.965221026022491,-0.261435213626798,0.));
#1743=DIRECTION('',(0.,0.,1.));
#1744=DIRECTION('center_axis',(-0.965221026022491,0.261435213626798,0.));
#1745=DIRECTION('ref_axis',(-0.261435213626798,-0.965221026022491,0.));
#1746=DIRECTION('',(0.261435213626798,0.965221026022491,0.));
#1747=DIRECTION('',(0.261435213626798,0.965221026022491,0.));
#1748=DIRECTION('',(0.,0.,-1.));
#1749=DIRECTION('center_axis',(0.261435213626798,0.965221026022491,0.));
#1750=DIRECTION('ref_axis',(-0.965221026022491,0.261435213626798,0.));
#1751=DIRECTION('',(-0.965221026022491,0.261435213626798,0.));
#1752=DIRECTION('',(-0.965221026022491,0.261435213626798,0.));
#1753=DIRECTION('',(0.,0.,1.));
#1754=DIRECTION('center_axis',(0.965221026022491,-0.261435213626797,0.));
#1755=DIRECTION('ref_axis',(0.261435213626797,0.965221026022491,0.));
#1756=DIRECTION('',(-0.261435213626797,-0.965221026022491,0.));
#1757=DIRECTION('',(-0.261435213626797,-0.965221026022491,0.));
#1758=DIRECTION('center_axis',(0.,0.,1.));
#1759=DIRECTION('ref_axis',(1.,0.,0.));
#1760=DIRECTION('center_axis',(0.,0.,1.));
#1761=DIRECTION('ref_axis',(-1.,0.,0.));
#1762=DIRECTION('axis',(0.,0.,1.));
#1763=DIRECTION('refdir',(1.,0.,0.));
#1764=DIRECTION('center_axis',(0.,0.,1.));
#1765=DIRECTION('ref_axis',(1.,0.,0.));
#1766=DIRECTION('center_axis',(0.,0.,1.));
#1767=DIRECTION('ref_axis',(1.,0.,0.));
#1768=DIRECTION('',(0.,0.,-1.));
#1769=DIRECTION('center_axis',(0.,0.,-1.));
#1770=DIRECTION('ref_axis',(1.,0.,0.));
#1771=DIRECTION('center_axis',(0.,0.,-1.));
#1772=DIRECTION('ref_axis',(1.,0.,0.));
#1773=DIRECTION('',(0.930484085528072,-1.13951435699951E-16,0.366332317137032));
#1774=DIRECTION('center_axis',(0.,0.,1.));
#1775=DIRECTION('ref_axis',(1.,0.,0.));
#1776=DIRECTION('center_axis',(0.,0.,1.));
#1777=DIRECTION('ref_axis',(1.,0.,0.));
#1778=DIRECTION('center_axis',(0.,0.,-1.));
#1779=DIRECTION('ref_axis',(-1.,0.,0.));
#1780=DIRECTION('axis',(0.,0.,1.));
#1781=DIRECTION('refdir',(1.,0.,0.));
#1782=DIRECTION('center_axis',(0.,0.,-1.));
#1783=DIRECTION('ref_axis',(-1.,0.,0.));
#1784=DIRECTION('center_axis',(0.,0.,-1.));
#1785=DIRECTION('ref_axis',(-1.,0.,0.));
#1786=DIRECTION('',(0.,0.,-1.));
#1787=DIRECTION('',(0.,0.,-1.));
#1788=DIRECTION('center_axis',(0.,7.40148683083438E-17,1.));
#1789=DIRECTION('ref_axis',(-1.,0.,0.));
#1790=DIRECTION('center_axis',(-1.,0.,0.));
#1791=DIRECTION('ref_axis',(0.,-1.,0.));
#1792=DIRECTION('center_axis',(-1.,0.,0.));
#1793=DIRECTION('ref_axis',(0.,-1.,0.));
#1794=DIRECTION('',(-1.,0.,0.));
#1795=DIRECTION('center_axis',(-1.,0.,0.));
#1796=DIRECTION('ref_axis',(0.,-1.,0.));
#1797=DIRECTION('',(0.,-1.,0.));
#1798=DIRECTION('',(0.,0.,-1.));
#1799=DIRECTION('',(0.,1.,-7.40148683083438E-17));
#1800=DIRECTION('',(0.,0.,1.));
#1801=DIRECTION('center_axis',(-1.,0.,0.));
#1802=DIRECTION('ref_axis',(0.,-1.,0.));
#1803=DIRECTION('',(-1.,0.,0.));
#1804=DIRECTION('center_axis',(1.,0.,0.));
#1805=DIRECTION('ref_axis',(0.,-1.,0.));
#1806=DIRECTION('center_axis',(0.,-1.,0.));
#1807=DIRECTION('ref_axis',(0.,0.,1.));
#1808=DIRECTION('',(1.,0.,0.));
#1809=DIRECTION('',(0.,0.,1.));
#1810=DIRECTION('',(-1.,0.,0.));
#1811=DIRECTION('center_axis',(0.,-7.40148683083438E-17,-1.));
#1812=DIRECTION('ref_axis',(0.,-1.,7.40148683083438E-17));
#1813=DIRECTION('',(0.,-1.,7.40148683083438E-17));
#1814=DIRECTION('',(-1.,0.,0.));
#1815=DIRECTION('center_axis',(0.,1.,0.));
#1816=DIRECTION('ref_axis',(0.,0.,-1.));
#1817=DIRECTION('',(0.,0.,-1.));
#1818=DIRECTION('',(-1.,0.,0.));
#1819=DIRECTION('center_axis',(0.,0.,1.));
#1820=DIRECTION('ref_axis',(0.,1.,0.));
#1821=DIRECTION('',(0.,1.,0.));
#1822=DIRECTION('center_axis',(-1.,0.,0.));
#1823=DIRECTION('ref_axis',(0.,-1.,0.));
#1824=DIRECTION('axis',(0.,0.,1.));
#1825=DIRECTION('refdir',(1.,0.,0.));
#1826=DIRECTION('center_axis',(1.,0.,0.));
#1827=DIRECTION('ref_axis',(0.,0.707106781186548,0.707106781186547));
#1828=DIRECTION('center_axis',(-1.,0.,0.));
#1829=DIRECTION('ref_axis',(0.,0.707106781186548,0.707106781186547));
#1830=DIRECTION('',(-1.,0.,0.));
#1831=DIRECTION('center_axis',(1.,0.,0.));
#1832=DIRECTION('ref_axis',(0.,0.707106781186548,0.707106781186547));
#1833=DIRECTION('',(1.,0.,0.));
#1834=DIRECTION('center_axis',(0.,0.,-1.));
#1835=DIRECTION('ref_axis',(-1.,0.,0.));
#1836=DIRECTION('',(0.,1.,0.));
#1837=DIRECTION('',(-1.,0.,0.));
#1838=DIRECTION('',(0.,-1.,0.));
#1839=DIRECTION('center_axis',(1.,0.,0.));
#1840=DIRECTION('ref_axis',(0.,0.,-1.));
#1841=DIRECTION('',(0.,0.,1.));
#1842=DIRECTION('',(0.,-1.,0.));
#1843=DIRECTION('',(0.,0.,-1.));
#1844=DIRECTION('center_axis',(1.,0.,0.));
#1845=DIRECTION('ref_axis',(0.,-0.707106781186548,0.707106781186547));
#1846=DIRECTION('center_axis',(-1.,0.,0.));
#1847=DIRECTION('ref_axis',(0.,-0.707106781186548,0.707106781186547));
#1848=DIRECTION('',(1.,0.,0.));
#1849=DIRECTION('center_axis',(-1.,0.,0.));
#1850=DIRECTION('ref_axis',(0.,-0.707106781186548,0.707106781186547));
#1851=DIRECTION('center_axis',(0.,-1.,0.));
#1852=DIRECTION('ref_axis',(0.,0.,1.));
#1853=DIRECTION('',(0.,0.,1.));
#1854=DIRECTION('',(-1.,0.,0.));
#1855=DIRECTION('',(0.,0.,1.));
#1856=DIRECTION('',(-1.,0.,0.));
#1857=DIRECTION('center_axis',(0.,0.,1.));
#1858=DIRECTION('ref_axis',(-0.707106781186544,-0.707106781186551,0.));
#1859=DIRECTION('center_axis',(0.,0.,-1.));
#1860=DIRECTION('ref_axis',(-0.707106781186544,-0.707106781186551,0.));
#1861=DIRECTION('',(0.,0.,-1.));
#1862=DIRECTION('center_axis',(0.,0.,1.));
#1863=DIRECTION('ref_axis',(-0.707106781186544,-0.707106781186551,0.));
#1864=DIRECTION('',(0.,0.,1.));
#1865=DIRECTION('center_axis',(0.,0.,-1.));
#1866=DIRECTION('ref_axis',(0.,-1.,0.));
#1867=DIRECTION('',(-1.,0.,0.));
#1868=DIRECTION('center_axis',(0.,0.,1.));
#1869=DIRECTION('ref_axis',(-0.707106781186544,0.707106781186551,0.));
#1870=DIRECTION('',(0.,-1.,0.));
#1871=DIRECTION('center_axis',(1.,0.,0.));
#1872=DIRECTION('ref_axis',(0.,0.,-1.));
#1873=DIRECTION('',(0.,0.,-1.));
#1874=DIRECTION('',(0.,1.,0.));
#1875=DIRECTION('center_axis',(0.,0.,-1.));
#1876=DIRECTION('ref_axis',(-0.707106781186544,0.707106781186551,0.));
#1877=DIRECTION('center_axis',(0.,0.,-1.));
#1878=DIRECTION('ref_axis',(-0.707106781186544,0.707106781186551,0.));
#1879=DIRECTION('center_axis',(1.,0.,0.));
#1880=DIRECTION('ref_axis',(0.,1.,0.));
#1881=DIRECTION('',(0.,0.,-1.));
#1882=DIRECTION('',(0.,1.,0.));
#1883=DIRECTION('center_axis',(0.,0.,1.));
#1884=DIRECTION('ref_axis',(0.,1.,0.));
#1885=DIRECTION('',(-1.,0.,0.));
#1886=DIRECTION('center_axis',(0.,1.,0.));
#1887=DIRECTION('ref_axis',(0.,0.,-1.));
#1888=DIRECTION('axis',(0.,0.,1.));
#1889=DIRECTION('refdir',(1.,0.,0.));
#1890=DIRECTION('center_axis',(-1.74459937578421E-17,-4.95164123815957E-15,
-1.));
#1891=DIRECTION('ref_axis',(1.,-6.93889390390722E-16,-1.74459937578387E-17));
#1892=DIRECTION('center_axis',(1.74459937578421E-17,4.95164123815957E-15,
1.));
#1893=DIRECTION('ref_axis',(-1.,0.,-2.92476088651957E-15));
#1894=DIRECTION('center_axis',(2.92476088651957E-15,0.,-1.));
#1895=DIRECTION('ref_axis',(-1.,0.,-3.0790185216271E-15));
#1896=DIRECTION('center_axis',(-2.92476088651957E-15,0.,1.));
#1897=DIRECTION('ref_axis',(1.,0.,2.92476088651957E-15));
#1898=DIRECTION('center_axis',(-1.22464679914735E-16,-1.,-3.58179905794757E-31));
#1899=DIRECTION('ref_axis',(1.,-1.22464679914735E-16,2.96059473233375E-15));
#1900=DIRECTION('center_axis',(2.92476088651957E-15,0.,-1.));
#1901=DIRECTION('ref_axis',(1.,0.,2.92476088651957E-15));
#1902=DIRECTION('center_axis',(-2.92476088651957E-15,0.,1.));
#1903=DIRECTION('ref_axis',(1.,0.,2.92476088651957E-15));
#1904=DIRECTION('',(-0.866025403784439,-0.5,-2.53291722772105E-15));
#1905=DIRECTION('',(-0.866025403784439,0.5,-2.53291722772105E-15));
#1906=DIRECTION('',(6.78692712841258E-16,1.,1.98501390048397E-30));
#1907=DIRECTION('',(0.866025403784439,0.5,2.53291722772105E-15));
#1908=DIRECTION('',(0.866025403784439,-0.5,2.53291722772105E-15));
#1909=DIRECTION('',(-1.1311545214021E-16,-1.,-3.30835650080662E-31));
#1910=DIRECTION('center_axis',(2.92476088651957E-15,0.,-1.));
#1911=DIRECTION('ref_axis',(-1.,0.,-2.92476088651957E-15));
#1912=DIRECTION('center_axis',(2.92476088651957E-15,0.,-1.));
#1913=DIRECTION('ref_axis',(1.,0.,2.92476088651957E-15));
#1914=DIRECTION('',(-2.92476088651957E-15,0.,1.));
#1915=DIRECTION('center_axis',(0.0435778713738291,-0.0754790873051733,-0.996194698091746));
#1916=DIRECTION('ref_axis',(-0.866025403784439,-0.5,-3.35810244624808E-17));
#1917=DIRECTION('',(3.18762329165829E-16,0.997141949694316,-0.0755508581011305));
#1918=DIRECTION('',(-0.866025403784439,-0.5,0.));
#1919=DIRECTION('',(-0.863550259614423,0.498570974847158,-0.0755508581011305));
#1920=DIRECTION('center_axis',(0.0871557427476581,-9.85866124751715E-18,
-0.996194698091746));
#1921=DIRECTION('ref_axis',(-1.1311545214021E-16,-1.,-2.40019600399866E-32));
#1922=DIRECTION('',(-1.1311545214021E-16,-1.,0.));
#1923=DIRECTION('',(-0.863550259614423,-0.498570974847158,-0.0755508581011305));
#1924=DIRECTION('center_axis',(0.0435778713738291,0.0754790873051733,-0.996194698091746));
#1925=DIRECTION('ref_axis',(0.866025403784439,-0.5,3.35810244624808E-17));
#1926=DIRECTION('',(0.866025403784439,-0.5,0.));
#1927=DIRECTION('',(-1.59381164582915E-16,-0.997141949694316,-0.0755508581011305));
#1928=DIRECTION('center_axis',(-0.043577871373829,0.0754790873051733,-0.996194698091746));
#1929=DIRECTION('ref_axis',(0.866025403784439,0.5,4.96857023844059E-17));
#1930=DIRECTION('',(0.866025403784439,0.5,0.));
#1931=DIRECTION('',(0.863550259614422,-0.498570974847159,-0.0755508581011305));
#1932=DIRECTION('center_axis',(-0.0871557427476581,5.91519674851029E-17,
-0.996194698091746));
#1933=DIRECTION('ref_axis',(6.78692712841258E-16,1.,4.0854062437599E-32));
#1934=DIRECTION('',(6.78692712841258E-16,1.,0.));
#1935=DIRECTION('',(0.863550259614423,0.498570974847158,-0.0755508581011305));
#1936=DIRECTION('center_axis',(-0.0435778713738291,-0.0754790873051733,
-0.996194698091746));
#1937=DIRECTION('ref_axis',(-0.866025403784439,0.5,3.35810244624808E-17));
#1938=DIRECTION('',(-0.866025403784438,0.5,0.));
#1939=DIRECTION('center_axis',(0.5,-0.866025403784439,0.));
#1940=DIRECTION('ref_axis',(-0.866025403784439,-0.5,0.));
#1941=DIRECTION('',(0.,0.,-1.));
#1942=DIRECTION('',(0.,0.,-1.));
#1943=DIRECTION('center_axis',(1.,-1.1311545214021E-16,0.));
#1944=DIRECTION('ref_axis',(-1.1311545214021E-16,-1.,0.));
#1945=DIRECTION('',(0.,0.,-1.));
#1946=DIRECTION('center_axis',(0.5,0.866025403784439,0.));
#1947=DIRECTION('ref_axis',(0.866025403784439,-0.5,0.));
#1948=DIRECTION('',(0.,0.,-1.));
#1949=DIRECTION('center_axis',(-0.5,0.866025403784439,0.));
#1950=DIRECTION('ref_axis',(0.866025403784439,0.5,0.));
#1951=DIRECTION('',(0.,0.,-1.));
#1952=DIRECTION('center_axis',(-1.,6.78692712841258E-16,0.));
#1953=DIRECTION('ref_axis',(6.78692712841258E-16,1.,0.));
#1954=DIRECTION('',(0.,0.,-1.));
#1955=DIRECTION('center_axis',(-0.5,-0.866025403784439,0.));
#1956=DIRECTION('ref_axis',(-0.866025403784439,0.5,0.));
#1957=DIRECTION('center_axis',(2.92476088651957E-15,0.,-1.));
#1958=DIRECTION('ref_axis',(-1.,0.,-2.92476088651957E-15));
#1959=DIRECTION('',(-2.92476088651957E-15,0.,1.));
#1960=DIRECTION('center_axis',(-2.92476088651957E-15,0.,1.));
#1961=DIRECTION('ref_axis',(-1.,0.,-2.92476088651957E-15));
#1962=DIRECTION('center_axis',(2.92476088651957E-15,0.,-1.));
#1963=DIRECTION('ref_axis',(-1.,0.,-2.92476088651957E-15));
#1964=DIRECTION('',(0.,0.,1.));
#1965=DIRECTION('',(1.,0.,0.));
#1966=DIRECTION('',(0.,0.,1.));
#1967=DIRECTION('',(1.,0.,0.));
#1968=DIRECTION('',(0.,0.,1.));
#1969=DIRECTION('',(1.,0.,0.));
#1970=DIRECTION('',(0.,0.,1.));
#1971=DIRECTION('',(1.,0.,0.));
#1972=DIRECTION('',(0.,0.,1.));
#1973=DIRECTION('',(1.,0.,0.));
#1974=DIRECTION('',(0.,0.,1.));
#1975=DIRECTION('',(1.,0.,0.));
#1976=DIRECTION('',(0.,0.,1.));
#1977=DIRECTION('',(1.,0.,0.));
#1978=DIRECTION('',(0.,0.,1.));
#1979=DIRECTION('',(1.,0.,0.));
#1980=DIRECTION('',(3.13237815656545E-17,0.,1.));
#1981=DIRECTION('',(0.999999999999997,6.93889390390723E-16,-1.38777878078115E-17));
#1982=DIRECTION('',(-3.0809194921309E-17,0.,1.));
#1983=DIRECTION('',(0.999999999999998,1.19348975147204E-15,3.74700270810993E-16));
#1984=CARTESIAN_POINT('',(0.,0.,0.));
#1985=CARTESIAN_POINT('',(0.,0.,0.));
#1986=CARTESIAN_POINT('Origin',(0.,0.,0.));
#1987=CARTESIAN_POINT('',(304.8,-8.,-9.79717439317883E-16));
#1988=CARTESIAN_POINT('Origin',(304.8,0.,0.));
#1989=CARTESIAN_POINT('',(0.,-8.,-9.79717439317883E-16));
#1990=CARTESIAN_POINT('',(0.,-8.,-9.79717439317883E-16));
#1991=CARTESIAN_POINT('Origin',(0.,0.,0.));
#1992=CARTESIAN_POINT('Origin',(304.8,0.,0.));
#1993=CARTESIAN_POINT('Origin',(0.,0.,0.));
#1994=CARTESIAN_POINT('',(0.,0.,0.));
#1995=CARTESIAN_POINT('Origin',(336.8,-17.,-16.25));
#1996=CARTESIAN_POINT('',(336.8,-20.,-20.));
#1997=CARTESIAN_POINT('',(339.8,-17.,-20.));
#1998=CARTESIAN_POINT('Origin',(336.8,-17.,-20.));
#1999=CARTESIAN_POINT('',(339.8,-17.,-15.));
#2000=CARTESIAN_POINT('',(339.8,-17.,-16.25));
#2001=CARTESIAN_POINT('',(336.8,-20.,-15.));
#2002=CARTESIAN_POINT('Origin',(336.8,-17.,-15.));
#2003=CARTESIAN_POINT('',(336.8,-20.,-16.25));
#2004=CARTESIAN_POINT('Origin',(304.8,20.,-15.));
#2005=CARTESIAN_POINT('',(339.8,17.,-15.));
#2006=CARTESIAN_POINT('',(339.8,20.,-15.));
#2007=CARTESIAN_POINT('',(336.8,20.,-15.));
#2008=CARTESIAN_POINT('Origin',(336.8,17.,-15.));
#2009=CARTESIAN_POINT('',(309.8,20.,-15.));
#2010=CARTESIAN_POINT('',(304.8,20.,-15.));
#2011=CARTESIAN_POINT('',(309.8,-20.,-15.));
#2012=CARTESIAN_POINT('',(309.8,10.,-15.));
#2013=CARTESIAN_POINT('',(304.8,-20.,-15.));
#2014=CARTESIAN_POINT('Origin',(339.8,0.,-17.5));
#2015=CARTESIAN_POINT('',(339.8,17.,-20.));
#2016=CARTESIAN_POINT('',(339.8,-20.,-20.));
#2017=CARTESIAN_POINT('',(339.8,17.,-18.75));
#2018=CARTESIAN_POINT('Origin',(336.8,17.,-18.75));
#2019=CARTESIAN_POINT('',(336.8,20.,-20.));
#2020=CARTESIAN_POINT('Origin',(336.8,17.,-20.));
#2021=CARTESIAN_POINT('',(336.8,20.,-18.75));
#2022=CARTESIAN_POINT('Origin',(304.8,17.,17.));
#2023=CARTESIAN_POINT('',(309.8,17.,20.));
#2024=CARTESIAN_POINT('',(309.8,20.,17.));
#2025=CARTESIAN_POINT('Origin',(309.8,17.,17.));
#2026=CARTESIAN_POINT('',(304.8,20.,17.));
#2027=CARTESIAN_POINT('',(304.8,20.,17.));
#2028=CARTESIAN_POINT('',(304.8,17.,20.));
#2029=CARTESIAN_POINT('Origin',(304.8,17.,17.));
#2030=CARTESIAN_POINT('',(304.8,17.,20.));
#2031=CARTESIAN_POINT('Origin',(304.8,20.,20.));
#2032=CARTESIAN_POINT('',(304.8,-17.,20.));
#2033=CARTESIAN_POINT('',(304.8,-20.,20.));
#2034=CARTESIAN_POINT('',(309.8,-17.,20.));
#2035=CARTESIAN_POINT('',(304.8,-17.,20.));
#2036=CARTESIAN_POINT('',(309.8,-20.,20.));
#2037=CARTESIAN_POINT('Origin',(304.8,0.,-17.5));
#2038=CARTESIAN_POINT('',(304.8,20.,-20.));
#2039=CARTESIAN_POINT('',(304.8,20.,-20.));
#2040=CARTESIAN_POINT('',(304.8,-20.,-20.));
#2041=CARTESIAN_POINT('',(304.8,-20.,-20.));
#2042=CARTESIAN_POINT('',(304.8,-20.,17.));
#2043=CARTESIAN_POINT('',(304.8,-20.,-15.));
#2044=CARTESIAN_POINT('Origin',(304.8,-17.,17.));
#2045=CARTESIAN_POINT('Origin',(304.8,-17.,17.));
#2046=CARTESIAN_POINT('',(309.8,-20.,17.));
#2047=CARTESIAN_POINT('Origin',(309.8,-17.,17.));
#2048=CARTESIAN_POINT('',(304.8,-20.,17.));
#2049=CARTESIAN_POINT('Origin',(309.8,0.,2.5));
#2050=CARTESIAN_POINT('',(309.8,-20.,-20.));
#2051=CARTESIAN_POINT('',(309.8,20.,20.));
#2052=CARTESIAN_POINT('Origin',(304.8,20.,-20.));
#2053=CARTESIAN_POINT('',(304.8,20.,-20.));
#2054=CARTESIAN_POINT('Origin',(304.8,-20.,-20.));
#2055=CARTESIAN_POINT('',(304.8,-20.,-20.));
#2056=CARTESIAN_POINT('Origin',(304.8,-20.,-15.));
#2057=CARTESIAN_POINT('',(0.,0.,0.));
#2058=CARTESIAN_POINT('Origin',(-205.724822686805,97.,19.9999999999958));
#2059=CARTESIAN_POINT('',(-195.724822686805,97.,14.9999999999958));
#2060=CARTESIAN_POINT('Origin',(-205.724822686805,97.,14.9999999999958));
#2061=CARTESIAN_POINT('',(-195.724822686805,97.,9.9999999999958));
#2062=CARTESIAN_POINT('',(-195.724822686805,97.,19.9999999999958));
#2063=CARTESIAN_POINT('Origin',(-205.724822686805,97.,9.9999999999958));
#2064=CARTESIAN_POINT('Origin',(-205.724822686805,97.,9.9999999999958));
#2065=CARTESIAN_POINT('Origin',(-205.724822686805,0.,14.9999999999958));
#2066=CARTESIAN_POINT('',(-78.724822686805,1.55530143491714E-14,14.9999999999958));
#2067=CARTESIAN_POINT('Origin',(-205.724822686805,0.,14.9999999999958));
#2068=CARTESIAN_POINT('',(-185.724822686805,-2.44929359829471E-15,14.9999999999958));
#2069=CARTESIAN_POINT('Origin',(-205.724822686805,0.,14.9999999999958));
#2070=CARTESIAN_POINT('Origin',(-205.724822686805,0.,0.));
#2071=CARTESIAN_POINT('',(-185.724822686805,2.44929359829471E-15,-10.));
#2072=CARTESIAN_POINT('',(-185.724822686805,-2.44929359829471E-15,0.));
#2073=CARTESIAN_POINT('Origin',(-205.724822686805,0.,-10.));
#2074=CARTESIAN_POINT('Origin',(-205.724822686805,0.,-10.));
#2075=CARTESIAN_POINT('Origin',(-205.724822686805,0.,-20.));
#2076=CARTESIAN_POINT('',(-78.7248226868051,1.55530143491714E-14,-12.));
#2077=CARTESIAN_POINT('',(-78.724822686805,1.55530143491714E-14,-20.));
#2078=CARTESIAN_POINT('Origin',(-205.724822686805,0.,-12.));
#2079=CARTESIAN_POINT('Origin',(-205.724822686805,0.,-12.));
#2080=CARTESIAN_POINT('',(0.,0.,0.));
#2081=CARTESIAN_POINT('Origin',(-205.724822686805,0.,-20.));
#2082=CARTESIAN_POINT('',(-53.3248226868051,-1.86636172190057E-14,-20.));
#2083=CARTESIAN_POINT('Origin',(-205.724822686805,0.,-20.));
#2084=CARTESIAN_POINT('',(-53.3248226868051,-1.86636172190057E-14,-35.));
#2085=CARTESIAN_POINT('',(-53.324822686805,-1.86636172190057E-14,-20.));
#2086=CARTESIAN_POINT('Origin',(-205.724822686805,0.,-35.));
#2087=CARTESIAN_POINT('Origin',(392.165319346077,-220.171232331321,-20.));
#2088=CARTESIAN_POINT('',(392.165319346077,-220.171232331321,-20.));
#2089=CARTESIAN_POINT('',(-392.165319346077,-220.171232331321,-20.));
#2090=CARTESIAN_POINT('',(392.165319346077,-220.171232331321,-20.));
#2091=CARTESIAN_POINT('',(-392.165319346077,-220.171232331321,-35.));
#2092=CARTESIAN_POINT('',(-392.165319346077,-220.171232331321,-20.));
#2093=CARTESIAN_POINT('',(392.165319346077,-220.171232331321,-35.));
#2094=CARTESIAN_POINT('',(392.165319346077,-220.171232331321,-35.));
#2095=CARTESIAN_POINT('',(392.165319346077,-220.171232331321,-20.));
#2096=CARTESIAN_POINT('Origin',(392.165319346077,220.171232331321,-20.));
#2097=CARTESIAN_POINT('',(392.165319346077,220.171232331321,-20.));
#2098=CARTESIAN_POINT('',(392.165319346077,220.171232331321,-20.));
#2099=CARTESIAN_POINT('',(392.165319346077,220.171232331321,-35.));
#2100=CARTESIAN_POINT('',(392.165319346077,220.171232331321,-35.));
#2101=CARTESIAN_POINT('',(392.165319346077,220.171232331321,-20.));
#2102=CARTESIAN_POINT('Origin',(-392.165319346077,220.171232331321,-20.));
#2103=CARTESIAN_POINT('',(-392.165319346077,220.171232331321,-20.));
#2104=CARTESIAN_POINT('',(-392.165319346077,220.171232331321,-20.));
#2105=CARTESIAN_POINT('',(-392.165319346077,220.171232331321,-35.));
#2106=CARTESIAN_POINT('',(-392.165319346077,220.171232331321,-35.));
#2107=CARTESIAN_POINT('',(-392.165319346077,220.171232331321,-20.));
#2108=CARTESIAN_POINT('Origin',(-392.165319346077,-220.171232331321,-20.));
#2109=CARTESIAN_POINT('',(-392.165319346077,-220.171232331321,-20.));
#2110=CARTESIAN_POINT('',(-392.165319346077,-220.171232331321,-35.));
#2111=CARTESIAN_POINT('Origin',(0.,0.,-35.));
#2112=CARTESIAN_POINT('Origin',(0.,0.,-20.));
#2113=CARTESIAN_POINT('',(0.,0.,0.));
#2114=CARTESIAN_POINT('Origin',(152.4,-2.52242671194836E-12,19.9999999999958));
#2115=CARTESIAN_POINT('',(162.4,-2.52120206514921E-12,19.9999999999958));
#2116=CARTESIAN_POINT('Origin',(152.4,-2.52242671194836E-12,19.9999999999958));
#2117=CARTESIAN_POINT('',(162.4,-2.52120206514921E-12,14.9999999999958));
#2118=CARTESIAN_POINT('',(162.4,-2.52365135874751E-12,19.9999999999958));
#2119=CARTESIAN_POINT('Origin',(152.4,-2.52242671194836E-12,14.9999999999958));
#2120=CARTESIAN_POINT('Origin',(-205.724822686805,97.,19.9999999999958));
#2121=CARTESIAN_POINT('',(-195.724822686805,97.,19.9999999999958));
#2122=CARTESIAN_POINT('Origin',(-205.724822686805,97.,19.9999999999958));
#2123=CARTESIAN_POINT('',(-195.724822686805,97.,14.9999999999958));
#2124=CARTESIAN_POINT('',(-195.724822686805,97.,19.9999999999958));
#2125=CARTESIAN_POINT('Origin',(-205.724822686805,97.,14.9999999999958));
#2126=CARTESIAN_POINT('Origin',(-212.260703027475,72.8694743494378,14.9999999999958));
#2127=CARTESIAN_POINT('',(169.994645309892,-30.6664059912348,14.9999999999958));
#2128=CARTESIAN_POINT('',(-241.21733380815,80.7125307582417,14.9999999999958));
#2129=CARTESIAN_POINT('',(145.86411965933,-24.1305256505648,14.9999999999958));
#2130=CARTESIAN_POINT('',(169.994645309892,-30.6664059912348,19.9999999999958));
#2131=CARTESIAN_POINT('',(169.994645309892,-30.6664059912348,14.9999999999958));
#2132=CARTESIAN_POINT('',(-241.21733380815,80.7125307582417,19.9999999999958));
#2133=CARTESIAN_POINT('',(145.86411965933,-24.1305256505648,19.9999999999958));
#2134=CARTESIAN_POINT('',(-241.21733380815,80.7125307582417,14.9999999999958));
#2135=CARTESIAN_POINT('Origin',(-228.14557312681,128.973582059366,14.9999999999958));
#2136=CARTESIAN_POINT('',(-228.14557312681,128.973582059366,14.9999999999958));
#2137=CARTESIAN_POINT('',(-231.413513297145,116.908319234085,14.9999999999958));
#2138=CARTESIAN_POINT('',(-228.14557312681,128.973582059366,19.9999999999958));
#2139=CARTESIAN_POINT('',(-231.413513297145,116.908319234085,19.9999999999958));
#2140=CARTESIAN_POINT('',(-228.14557312681,128.973582059366,14.9999999999958));
#2141=CARTESIAN_POINT('Origin',(158.93588034067,24.1305256505598,14.9999999999958));
#2142=CARTESIAN_POINT('',(183.066405991232,17.5946453098898,14.9999999999958));
#2143=CARTESIAN_POINT('',(158.93588034067,24.1305256505598,14.9999999999958));
#2144=CARTESIAN_POINT('',(183.066405991232,17.5946453098898,19.9999999999958));
#2145=CARTESIAN_POINT('',(158.93588034067,24.1305256505598,19.9999999999958));
#2146=CARTESIAN_POINT('',(183.066405991232,17.5946453098898,14.9999999999958));
#2147=CARTESIAN_POINT('Origin',(169.994645309892,-30.6664059912347,14.9999999999958));
#2148=CARTESIAN_POINT('',(173.262585480227,-18.6011431659535,14.9999999999958));
#2149=CARTESIAN_POINT('',(173.262585480227,-18.6011431659535,19.9999999999958));
#2150=CARTESIAN_POINT('Origin',(-26.6624113434025,48.4999999999987,19.9999999999958));
#2151=CARTESIAN_POINT('Origin',(-26.6624113434025,48.4999999999987,14.9999999999958));
#2152=CARTESIAN_POINT('',(0.,0.,0.));
#2153=CARTESIAN_POINT('Origin',(-205.724822686805,0.,-24.5));
#2154=CARTESIAN_POINT('',(-358.124822686805,-1.86636172190057E-14,-22.));
#2155=CARTESIAN_POINT('Origin',(-205.724822686805,0.,-22.));
#2156=CARTESIAN_POINT('',(-358.124822686805,1.86636172190057E-14,-35.));
#2157=CARTESIAN_POINT('',(-358.124822686805,-1.86636172190057E-14,-24.5));
#2158=CARTESIAN_POINT('Origin',(-205.724822686805,0.,-35.));
#2159=CARTESIAN_POINT('Origin',(-205.724822686805,0.,-17.));
#2160=CARTESIAN_POINT('',(-332.724822686805,-1.55530143491714E-14,-12.));
#2161=CARTESIAN_POINT('',(-345.424822686805,1.71083157840885E-14,-17.));
#2162=CARTESIAN_POINT('Origin',(-205.724822686805,0.,-12.));
#2163=CARTESIAN_POINT('Origin',(-205.724822686805,0.,-12.));
#2164=CARTESIAN_POINT('Origin',(-53.3248226868051,0.,-35.));
#2165=CARTESIAN_POINT('',(0.,0.,0.));
#2166=CARTESIAN_POINT('Origin',(152.4,-2.52242671194836E-12,14.9999999999958));
#2167=CARTESIAN_POINT('',(162.29525,-2.52121489332443E-12,14.9999999999958));
#2168=CARTESIAN_POINT('Origin',(152.4,-2.52242671194836E-12,14.9999999999958));
#2169=CARTESIAN_POINT('',(162.29525,-1.26161109846903E-12,8.));
#2170=CARTESIAN_POINT('',(162.29525,-2.52363853057229E-12,14.9999999999958));
#2171=CARTESIAN_POINT('',(162.29525,-1.26119476483479E-12,-8.));
#2172=CARTESIAN_POINT('Ctrl Pts',(162.29525,1.66533453693773E-15,-8.));
#2173=CARTESIAN_POINT('Ctrl Pts',(162.29525,-1.06114689645934,-8.));
#2174=CARTESIAN_POINT('Ctrl Pts',(162.112073508216,-2.15862639679729,-7.77661292309447));
#2175=CARTESIAN_POINT('Ctrl Pts',(161.456447542343,-4.11883390373875,-6.9405026969991));
#2176=CARTESIAN_POINT('Ctrl Pts',(160.987841858536,-4.9837667164534,-6.32994178253133));
#2177=CARTESIAN_POINT('Ctrl Pts',(160.033751169964,-6.35310263577037,-4.96060586321443));
#2178=CARTESIAN_POINT('Ctrl Pts',(159.469158415985,-6.95125183484192,-4.09614535763875));
#2179=CARTESIAN_POINT('Ctrl Pts',(158.784045152537,-7.56664871511797,-2.64960450672535));
#2180=CARTESIAN_POINT('Ctrl Pts',(158.584436338924,-7.7265896208107,-2.14179168027124));
#2181=CARTESIAN_POINT('Ctrl Pts',(158.303524359677,-7.94328901302828,-1.09161265583592));
#2182=CARTESIAN_POINT('Ctrl Pts',(158.223742144235,-8.,-0.548830410606655));
#2183=CARTESIAN_POINT('Ctrl Pts',(158.223742144235,-8.,0.548830410606653));
#2184=CARTESIAN_POINT('Ctrl Pts',(158.303524359677,-7.94328901302828,1.09161265583591));
#2185=CARTESIAN_POINT('Ctrl Pts',(158.584436338924,-7.7265896208107,2.14179168027124));
#2186=CARTESIAN_POINT('Ctrl Pts',(158.784045152537,-7.56664871511797,2.64960450672535));
#2187=CARTESIAN_POINT('Ctrl Pts',(159.469158415985,-6.95125183484192,4.09614535763875));
#2188=CARTESIAN_POINT('Ctrl Pts',(160.033751169964,-6.35310263577037,4.96060586321443));
#2189=CARTESIAN_POINT('Ctrl Pts',(160.987841858536,-4.98376671645341,6.32994178253132));
#2190=CARTESIAN_POINT('Ctrl Pts',(161.456447542343,-4.11883390373875,6.94050269699909));
#2191=CARTESIAN_POINT('Ctrl Pts',(162.112073508216,-2.15862639679729,7.77661292309447));
#2192=CARTESIAN_POINT('Ctrl Pts',(162.29525,-1.06114689645934,8.));
#2193=CARTESIAN_POINT('Ctrl Pts',(162.29525,-1.94289029309402E-15,8.));
#2194=CARTESIAN_POINT('',(162.29525,-2.52121489332443E-12,-15.0000000000042));
#2195=CARTESIAN_POINT('',(162.29525,-2.52363853057229E-12,14.9999999999958));
#2196=CARTESIAN_POINT('Origin',(152.4,-2.52242671194836E-12,-15.0000000000042));
#2197=CARTESIAN_POINT('',(158.223742144228,8.,-4.16333634234434E-16));
#2198=CARTESIAN_POINT('Ctrl Pts',(158.223742144228,8.,-4.16333634234434E-16));
#2199=CARTESIAN_POINT('Ctrl Pts',(158.223742144228,8.,-0.548830410606754));
#2200=CARTESIAN_POINT('Ctrl Pts',(158.30352435967,7.94328901302826,-1.09161265583602));
#2201=CARTESIAN_POINT('Ctrl Pts',(158.584436338918,7.72658962081068,-2.1417916802713));
#2202=CARTESIAN_POINT('Ctrl Pts',(158.784045152531,7.56664871511797,-2.64960450672535));
#2203=CARTESIAN_POINT('Ctrl Pts',(159.46915841598,6.951251834842,-4.09614535763859));
#2204=CARTESIAN_POINT('Ctrl Pts',(160.03375116996,6.35310263577055,-4.96060586321418));
#2205=CARTESIAN_POINT('Ctrl Pts',(160.987841858533,4.98376671645374,-6.32994178253105));
#2206=CARTESIAN_POINT('Ctrl Pts',(161.45644754234,4.11883390373914,-6.94050269699888));
#2207=CARTESIAN_POINT('Ctrl Pts',(162.112073508215,2.1586263967976,-7.77661292309439));
#2208=CARTESIAN_POINT('Ctrl Pts',(162.29525,1.06114689645957,-8.));
#2209=CARTESIAN_POINT('Ctrl Pts',(162.29525,1.52655665885959E-15,-8.));
#2210=CARTESIAN_POINT('Ctrl Pts',(162.29525,5.55111512312578E-16,8.));
#2211=CARTESIAN_POINT('Ctrl Pts',(162.29525,1.06114689645957,8.));
#2212=CARTESIAN_POINT('Ctrl Pts',(162.112073508215,2.1586263967976,7.77661292309439));
#2213=CARTESIAN_POINT('Ctrl Pts',(161.45644754234,4.11883390373913,6.94050269699888));
#2214=CARTESIAN_POINT('Ctrl Pts',(160.987841858533,4.98376671645374,6.32994178253105));
#2215=CARTESIAN_POINT('Ctrl Pts',(160.03375116996,6.35310263577055,4.96060586321418));
#2216=CARTESIAN_POINT('Ctrl Pts',(159.46915841598,6.951251834842,4.09614535763859));
#2217=CARTESIAN_POINT('Ctrl Pts',(158.784045152531,7.56664871511797,2.64960450672535));
#2218=CARTESIAN_POINT('Ctrl Pts',(158.584436338918,7.72658962081068,2.1417916802713));
#2219=CARTESIAN_POINT('Ctrl Pts',(158.30352435967,7.94328901302826,1.09161265583602));
#2220=CARTESIAN_POINT('Ctrl Pts',(158.223742144228,8.,0.548830410606755));
#2221=CARTESIAN_POINT('Ctrl Pts',(158.223742144228,8.,1.11022302462516E-15));
#2222=CARTESIAN_POINT('',(146.576257855772,8.,2.77555756156289E-16));
#2223=CARTESIAN_POINT('Ctrl Pts',(146.576257855772,8.,2.77555756156289E-16));
#2224=CARTESIAN_POINT('Ctrl Pts',(146.576257855772,8.,0.548830410606754));
#2225=CARTESIAN_POINT('Ctrl Pts',(146.49647564033,7.94328901302826,1.09161265583602));
#2226=CARTESIAN_POINT('Ctrl Pts',(146.215563661082,7.72658962081068,2.1417916802713));
#2227=CARTESIAN_POINT('Ctrl Pts',(146.015954847468,7.56664871511797,2.64960450672535));
#2228=CARTESIAN_POINT('Ctrl Pts',(145.33084158402,6.951251834842,4.09614535763859));
#2229=CARTESIAN_POINT('Ctrl Pts',(144.76624883004,6.35310263577055,4.96060586321418));
#2230=CARTESIAN_POINT('Ctrl Pts',(143.812158141467,4.98376671645374,6.32994178253105));
#2231=CARTESIAN_POINT('Ctrl Pts',(143.34355245766,4.11883390373914,6.94050269699888));
#2232=CARTESIAN_POINT('Ctrl Pts',(142.687926491785,2.15862639679761,7.77661292309439));
#2233=CARTESIAN_POINT('Ctrl Pts',(142.50475,1.06114689645956,8.));
#2234=CARTESIAN_POINT('Ctrl Pts',(142.50475,-1.06114689645934,8.));
#2235=CARTESIAN_POINT('Ctrl Pts',(142.687926491784,-2.15862639679729,7.77661292309447));
#2236=CARTESIAN_POINT('Ctrl Pts',(143.343552457657,-4.11883390373876,6.94050269699909));
#2237=CARTESIAN_POINT('Ctrl Pts',(143.812158141464,-4.98376671645341,6.32994178253132));
#2238=CARTESIAN_POINT('Ctrl Pts',(144.766248830036,-6.35310263577037,4.96060586321443));
#2239=CARTESIAN_POINT('Ctrl Pts',(145.330841584015,-6.95125183484192,4.09614535763875));
#2240=CARTESIAN_POINT('Ctrl Pts',(146.015954847463,-7.56664871511797,2.64960450672535));
#2241=CARTESIAN_POINT('Ctrl Pts',(146.215563661076,-7.7265896208107,2.14179168027124));
#2242=CARTESIAN_POINT('Ctrl Pts',(146.496475640323,-7.94328901302828,1.09161265583591));
#2243=CARTESIAN_POINT('Ctrl Pts',(146.576257855765,-8.,0.548830410606653));
#2244=CARTESIAN_POINT('Ctrl Pts',(146.576257855765,-8.,-0.548830410606655));
#2245=CARTESIAN_POINT('Ctrl Pts',(146.496475640323,-7.94328901302828,-1.09161265583592));
#2246=CARTESIAN_POINT('Ctrl Pts',(146.215563661076,-7.7265896208107,-2.14179168027124));
#2247=CARTESIAN_POINT('Ctrl Pts',(146.015954847463,-7.56664871511797,-2.64960450672535));
#2248=CARTESIAN_POINT('Ctrl Pts',(145.330841584015,-6.95125183484192,-4.09614535763875));
#2249=CARTESIAN_POINT('Ctrl Pts',(144.766248830036,-6.35310263577037,-4.96060586321443));
#2250=CARTESIAN_POINT('Ctrl Pts',(143.812158141464,-4.9837667164534,-6.32994178253133));
#2251=CARTESIAN_POINT('Ctrl Pts',(143.343552457657,-4.11883390373876,-6.94050269699909));
#2252=CARTESIAN_POINT('Ctrl Pts',(142.687926491784,-2.15862639679729,-7.77661292309447));
#2253=CARTESIAN_POINT('Ctrl Pts',(142.50475,-1.06114689645934,-8.));
#2254=CARTESIAN_POINT('Ctrl Pts',(142.50475,1.06114689645956,-8.));
#2255=CARTESIAN_POINT('Ctrl Pts',(142.687926491785,2.15862639679761,-7.77661292309439));
#2256=CARTESIAN_POINT('Ctrl Pts',(143.34355245766,4.11883390373914,-6.94050269699887));
#2257=CARTESIAN_POINT('Ctrl Pts',(143.812158141467,4.98376671645374,-6.32994178253105));
#2258=CARTESIAN_POINT('Ctrl Pts',(144.76624883004,6.35310263577055,-4.96060586321418));
#2259=CARTESIAN_POINT('Ctrl Pts',(145.33084158402,6.951251834842,-4.09614535763859));
#2260=CARTESIAN_POINT('Ctrl Pts',(146.015954847468,7.56664871511797,-2.64960450672535));
#2261=CARTESIAN_POINT('Ctrl Pts',(146.215563661082,7.72658962081068,-2.1417916802713));
#2262=CARTESIAN_POINT('Ctrl Pts',(146.49647564033,7.94328901302826,-1.09161265583602));
#2263=CARTESIAN_POINT('Ctrl Pts',(146.576257855772,8.,-0.54883041060675));
#2264=CARTESIAN_POINT('Ctrl Pts',(146.576257855772,8.,3.53883589099269E-15));
#2265=CARTESIAN_POINT('Origin',(152.4,0.,0.));
#2266=CARTESIAN_POINT('',(177.4,8.,-9.79717439317883E-16));
#2267=CARTESIAN_POINT('Origin',(177.4,0.,0.));
#2268=CARTESIAN_POINT('',(152.4,8.,-9.79717439317883E-16));
#2269=CARTESIAN_POINT('Origin',(177.4,-2.52686760404686E-12,-4.20552481728009E-12));
#2270=CARTESIAN_POINT('',(177.4,14.9999999999975,14.9999999999958));
#2271=CARTESIAN_POINT('',(177.4,-15.0000000000025,14.9999999999958));
#2272=CARTESIAN_POINT('',(177.4,14.9999999999975,14.9999999999958));
#2273=CARTESIAN_POINT('',(177.4,-15.0000000000025,-15.0000000000042));
#2274=CARTESIAN_POINT('',(177.4,-15.0000000000025,14.9999999999958));
#2275=CARTESIAN_POINT('',(177.4,14.9999999999975,-15.0000000000042));
#2276=CARTESIAN_POINT('',(177.4,-15.0000000000025,-15.0000000000042));
#2277=CARTESIAN_POINT('',(177.4,14.9999999999975,-15.0000000000042));
#2278=CARTESIAN_POINT('Origin',(152.4,0.,0.));
#2279=CARTESIAN_POINT('',(127.4,8.,-9.79717439317883E-16));
#2280=CARTESIAN_POINT('',(152.4,8.,-9.79717439317883E-16));
#2281=CARTESIAN_POINT('Origin',(127.4,0.,0.));
#2282=CARTESIAN_POINT('Origin',(152.4,-15.0000000000025,-15.0000000000042));
#2283=CARTESIAN_POINT('',(127.4,-15.0000000000025,14.9999999999958));
#2284=CARTESIAN_POINT('',(152.4,-15.0000000000025,14.9999999999958));
#2285=CARTESIAN_POINT('',(127.4,-15.0000000000025,-15.0000000000042));
#2286=CARTESIAN_POINT('',(127.4,-15.0000000000025,14.9999999999958));
#2287=CARTESIAN_POINT('',(152.4,-15.0000000000025,-15.0000000000042));
#2288=CARTESIAN_POINT('Origin',(152.4,14.9999999999975,-15.0000000000042));
#2289=CARTESIAN_POINT('',(127.4,14.9999999999975,-15.0000000000042));
#2290=CARTESIAN_POINT('',(127.4,-15.0000000000025,-15.0000000000042));
#2291=CARTESIAN_POINT('',(152.4,14.9999999999975,-15.0000000000042));
#2292=CARTESIAN_POINT('Origin',(152.4,14.9999999999975,14.9999999999958));
#2293=CARTESIAN_POINT('',(127.4,14.9999999999975,14.9999999999958));
#2294=CARTESIAN_POINT('',(127.4,14.9999999999975,-15.0000000000042));
#2295=CARTESIAN_POINT('',(152.4,14.9999999999975,14.9999999999958));
#2296=CARTESIAN_POINT('Origin',(152.4,-15.0000000000025,14.9999999999958));
#2297=CARTESIAN_POINT('',(127.4,14.9999999999975,14.9999999999958));
#2298=CARTESIAN_POINT('Origin',(127.4,-2.52686760404686E-12,-4.20552481728009E-12));
#2299=CARTESIAN_POINT('',(0.,0.,0.));
#2300=CARTESIAN_POINT('Origin',(0.,18.,9.43656992056115));
#2301=CARTESIAN_POINT('',(0.,18.,11.4365699205612));
#2302=CARTESIAN_POINT('',(0.,20.,9.43656992056115));
#2303=CARTESIAN_POINT('Origin',(0.,18.,9.43656992056115));
#2304=CARTESIAN_POINT('',(-5.,20.,9.43656992056115));
#2305=CARTESIAN_POINT('',(0.,20.,9.43656992056115));
#2306=CARTESIAN_POINT('',(-5.,18.,11.4365699205612));
#2307=CARTESIAN_POINT('Origin',(-5.,18.,9.43656992056115));
#2308=CARTESIAN_POINT('',(0.,18.,11.4365699205612));
#2309=CARTESIAN_POINT('Origin',(0.,-20.,11.4365699205612));
#2310=CARTESIAN_POINT('',(-5.,-18.,11.4365699205612));
#2311=CARTESIAN_POINT('',(-5.,-10.,11.4365699205612));
#2312=CARTESIAN_POINT('',(0.,-18.,11.4365699205612));
#2313=CARTESIAN_POINT('',(0.,-18.,11.4365699205612));
#2314=CARTESIAN_POINT('',(0.,-10.,11.4365699205612));
#2315=CARTESIAN_POINT('Origin',(-5.,0.,2.5));
#2316=CARTESIAN_POINT('',(-5.,20.,-15.));
#2317=CARTESIAN_POINT('',(-5.,20.,20.));
#2318=CARTESIAN_POINT('',(-5.,-20.,-15.));
#2319=CARTESIAN_POINT('',(-5.,10.,-15.));
#2320=CARTESIAN_POINT('',(-5.,-20.,9.43656992056115));
#2321=CARTESIAN_POINT('',(-5.,-20.,-20.));
#2322=CARTESIAN_POINT('Origin',(-5.,-18.,9.43656992056115));
#2323=CARTESIAN_POINT('Origin',(0.,-18.,9.43656992056115));
#2324=CARTESIAN_POINT('',(0.,-20.,9.43656992056115));
#2325=CARTESIAN_POINT('',(0.,-20.,9.43656992056115));
#2326=CARTESIAN_POINT('Origin',(0.,-18.,9.43656992056115));
#2327=CARTESIAN_POINT('Origin',(0.,20.,-20.));
#2328=CARTESIAN_POINT('',(0.,20.,-20.));
#2329=CARTESIAN_POINT('',(0.,20.,-20.));
#2330=CARTESIAN_POINT('',(-32.0000000000001,20.,-20.));
#2331=CARTESIAN_POINT('',(0.,20.,-20.));
#2332=CARTESIAN_POINT('',(-32.0000000000001,20.,-15.));
#2333=CARTESIAN_POINT('',(-32.0000000000001,20.,-18.75));
#2334=CARTESIAN_POINT('',(0.,20.,-15.));
#2335=CARTESIAN_POINT('Origin',(-32.0000000000001,-17.,-16.25));
#2336=CARTESIAN_POINT('',(-32.0000000000001,-20.,-20.));
#2337=CARTESIAN_POINT('',(-35.,-17.,-20.));
#2338=CARTESIAN_POINT('Origin',(-32.0000000000001,-17.,-20.));
#2339=CARTESIAN_POINT('',(-32.0000000000001,-20.,-15.));
#2340=CARTESIAN_POINT('',(-32.0000000000001,-20.,-16.25));
#2341=CARTESIAN_POINT('',(-35.,-17.,-15.));
#2342=CARTESIAN_POINT('Origin',(-32.0000000000001,-17.,-15.));
#2343=CARTESIAN_POINT('',(-35.,-17.,-16.25));
#2344=CARTESIAN_POINT('Origin',(0.,20.,-15.));
#2345=CARTESIAN_POINT('',(0.,-20.,-15.));
#2346=CARTESIAN_POINT('',(-35.,17.,-15.));
#2347=CARTESIAN_POINT('Origin',(-32.0000000000001,17.,-15.));
#2348=CARTESIAN_POINT('',(-35.,20.,-15.));
#2349=CARTESIAN_POINT('Origin',(-35.,0.,-17.5));
#2350=CARTESIAN_POINT('',(-35.,17.,-20.));
#2351=CARTESIAN_POINT('',(-35.,17.,-18.75));
#2352=CARTESIAN_POINT('',(-35.,-20.,-20.));
#2353=CARTESIAN_POINT('Origin',(-32.0000000000001,17.,-18.75));
#2354=CARTESIAN_POINT('Origin',(-32.0000000000001,17.,-20.));
#2355=CARTESIAN_POINT('Origin',(0.,0.,-17.5));
#2356=CARTESIAN_POINT('',(0.,-20.,-20.));
#2357=CARTESIAN_POINT('',(0.,-20.,-15.));
#2358=CARTESIAN_POINT('',(0.,-20.,-20.));
#2359=CARTESIAN_POINT('Origin',(0.,-20.,-20.));
#2360=CARTESIAN_POINT('',(0.,-20.,-20.));
#2361=CARTESIAN_POINT('Origin',(0.,-20.,-15.));
#2362=CARTESIAN_POINT('',(0.,0.,0.));
#2363=CARTESIAN_POINT('Origin',(-1.4210854715202E-13,3.00426815946881E-13,
-10.0000000000003));
#2364=CARTESIAN_POINT('',(9.89524999999999,-1.21181862392628E-15,-10.0000000000004));
#2365=CARTESIAN_POINT('Origin',(-7.97007865091842E-15,0.,-10.0000000000003));
#2366=CARTESIAN_POINT('Origin',(-8.98633834734665E-14,0.,17.9999999999997));
#2367=CARTESIAN_POINT('',(14.9999999999999,-1.83697019872103E-15,17.9999999999997));
#2368=CARTESIAN_POINT('Origin',(-8.98633834734665E-14,0.,17.9999999999997));
#2369=CARTESIAN_POINT('',(12.9999999999999,-1.59204083889156E-15,19.9999999999997));
#2370=CARTESIAN_POINT('Origin',(12.9999999999999,-1.59204083889156E-15,
17.9999999999997));
#2371=CARTESIAN_POINT('Origin',(-9.57129052465056E-14,0.,19.9999999999997));
#2372=CARTESIAN_POINT('Origin',(-15.0000000000001,0.,19.9999999999996));
#2373=CARTESIAN_POINT('',(8.5,-4.90747728811182,20.));
#2374=CARTESIAN_POINT('',(3.33066907387547E-15,-9.81495457622364,20.));
#2375=CARTESIAN_POINT('',(0.749999999999985,-9.38194187433143,19.9999999999997));
#2376=CARTESIAN_POINT('',(-8.50000000000001,-4.90747728811181,20.));
#2377=CARTESIAN_POINT('',(-7.75000000000002,-5.34048999000403,19.9999999999997));
#2378=CARTESIAN_POINT('',(-8.5,4.90747728811182,20.));
#2379=CARTESIAN_POINT('',(-8.50000000000001,-2.45373864405591,19.9999999999997));
#2380=CARTESIAN_POINT('',(1.12757025938492E-15,9.81495457622364,20.));
#2381=CARTESIAN_POINT('',(-12.,2.88675134594812,19.9999999999997));
#2382=CARTESIAN_POINT('',(8.5,4.90747728811182,20.));
#2383=CARTESIAN_POINT('',(-3.50000000000002,11.8356805183873,19.9999999999997));
#2384=CARTESIAN_POINT('',(8.5,2.45373864405591,19.9999999999997));
#2385=CARTESIAN_POINT('Origin',(-6.64652963813099E-14,0.,9.99999999999969));
#2386=CARTESIAN_POINT('',(14.9999999999999,-1.83697019872103E-15,-2.67563748934663E-13));
#2387=CARTESIAN_POINT('Origin',(-3.72176875161141E-14,0.,-3.1184928405981E-13));
#2388=CARTESIAN_POINT('',(14.9999999999999,-1.83697019872103E-15,9.99999999999973));
#2389=CARTESIAN_POINT('Origin',(3.33066907387547E-15,-9.81495457622364,
10.));
#2390=CARTESIAN_POINT('',(3.33066907387547E-15,-9.81495457622364,10.));
#2391=CARTESIAN_POINT('',(-9.72987853259607E-16,-2.22044604925031E-15,9.25634636002965));
#2392=CARTESIAN_POINT('',(-3.33066907387547E-15,-7.37522170588592,9.81514777113925));
#2393=CARTESIAN_POINT('',(8.5,-4.90747728811182,10.));
#2394=CARTESIAN_POINT('',(3.19337359890869E-15,-9.81495457622364,10.));
#2395=CARTESIAN_POINT('',(6.38712935583962,-3.68761085294296,9.81514777113925));
#2396=CARTESIAN_POINT('Origin',(8.5,-4.90747728811182,10.));
#2397=CARTESIAN_POINT('',(8.5,4.90747728811182,10.));
#2398=CARTESIAN_POINT('',(8.5,-4.90747728811182,10.));
#2399=CARTESIAN_POINT('',(6.38712935583961,3.68761085294296,9.81514777113925));
#2400=CARTESIAN_POINT('Origin',(8.5,4.90747728811182,10.));
#2401=CARTESIAN_POINT('',(1.11022302462516E-15,9.81495457622364,10.));
#2402=CARTESIAN_POINT('',(8.5,4.90747728811182,10.));
#2403=CARTESIAN_POINT('',(-2.22044604925031E-15,7.37522170588592,9.81514777113925));
#2404=CARTESIAN_POINT('Origin',(1.11022302462516E-15,9.81495457622364,10.));
#2405=CARTESIAN_POINT('',(-8.5,4.90747728811182,10.));
#2406=CARTESIAN_POINT('',(1.12757025938492E-15,9.81495457622364,10.));
#2407=CARTESIAN_POINT('',(-6.38712935583961,3.68761085294296,9.81514777113925));
#2408=CARTESIAN_POINT('Origin',(-8.5,4.90747728811182,10.));
#2409=CARTESIAN_POINT('',(-8.50000000000001,-4.90747728811181,10.));
#2410=CARTESIAN_POINT('',(-8.5,4.90747728811182,10.));
#2411=CARTESIAN_POINT('',(-6.38712935583962,-3.68761085294295,9.81514777113925));
#2412=CARTESIAN_POINT('Origin',(-8.50000000000001,-4.90747728811181,10.));
#2413=CARTESIAN_POINT('',(-8.50000000000001,-4.90747728811181,10.));
#2414=CARTESIAN_POINT('Origin',(8.5,-4.90747728811182,20.));
#2415=CARTESIAN_POINT('',(8.5,-4.90747728811182,20.));
#2416=CARTESIAN_POINT('',(3.33066907387547E-15,-9.81495457622364,20.));
#2417=CARTESIAN_POINT('Origin',(8.5,4.90747728811182,20.));
#2418=CARTESIAN_POINT('',(8.5,4.90747728811182,20.));
#2419=CARTESIAN_POINT('Origin',(1.11022302462516E-15,9.81495457622364,20.));
#2420=CARTESIAN_POINT('',(1.12757025938492E-15,9.81495457622364,20.));
#2421=CARTESIAN_POINT('Origin',(-8.5,4.90747728811182,20.));
#2422=CARTESIAN_POINT('',(-8.5,4.90747728811182,20.));
#2423=CARTESIAN_POINT('Origin',(-8.50000000000001,-4.90747728811181,20.));
#2424=CARTESIAN_POINT('',(-8.50000000000001,-4.90747728811181,20.));
#2425=CARTESIAN_POINT('Origin',(3.33066907387547E-15,-9.81495457622364,
20.));
#2426=CARTESIAN_POINT('Origin',(-7.9700786509191E-15,0.,-10.0000000000001));
#2427=CARTESIAN_POINT('',(9.89524999999996,1.21181862392628E-15,-1.32099810487998E-13));
#2428=CARTESIAN_POINT('',(9.89524999999999,-1.21181862392628E-15,-10.0000000000001));
#2429=CARTESIAN_POINT('Origin',(-3.72176875161146E-14,0.,-1.60982338570648E-13));
#2430=CARTESIAN_POINT('Origin',(-10.,0.,-1.89717705257387E-13));
#2431=CARTESIAN_POINT('',(0.,0.,0.));
#2432=CARTESIAN_POINT('',(0.,0.,0.));
#2433=CARTESIAN_POINT('',(0.,0.,0.));
#2434=CARTESIAN_POINT('',(0.,0.,0.));
#2435=CARTESIAN_POINT('',(0.,0.,0.));
#2436=CARTESIAN_POINT('',(0.,0.,0.));
#2437=CARTESIAN_POINT('',(0.,0.,0.));
#2438=CARTESIAN_POINT('',(0.,0.,0.));
#2439=CARTESIAN_POINT('',(152.4,-2.57571741713037E-12,19.999999999996));
#2440=CARTESIAN_POINT('',(-205.724822686805,97.,19.9999999999961));
#2441=UNCERTAINTY_MEASURE_WITH_UNIT(LENGTH_MEASURE(0.01),#2463,
'DISTANCE_ACCURACY_VALUE',
'Maximum model space distance between geometric entities at asserted c
onnectivities');
#2442=UNCERTAINTY_MEASURE_WITH_UNIT(LENGTH_MEASURE(0.01),#2463,
'DISTANCE_ACCURACY_VALUE',
'Maximum model space distance between geometric entities at asserted c
onnectivities');
#2443=UNCERTAINTY_MEASURE_WITH_UNIT(LENGTH_MEASURE(0.01),#2463,
'DISTANCE_ACCURACY_VALUE',
'Maximum model space distance between geometric entities at asserted c
onnectivities');
#2444=UNCERTAINTY_MEASURE_WITH_UNIT(LENGTH_MEASURE(0.01),#2463,
'DISTANCE_ACCURACY_VALUE',
'Maximum model space distance between geometric entities at asserted c
onnectivities');
#2445=UNCERTAINTY_MEASURE_WITH_UNIT(LENGTH_MEASURE(0.01),#2463,
'DISTANCE_ACCURACY_VALUE',
'Maximum model space distance between geometric entities at asserted c
onnectivities');
#2446=UNCERTAINTY_MEASURE_WITH_UNIT(LENGTH_MEASURE(0.01),#2463,
'DISTANCE_ACCURACY_VALUE',
'Maximum model space distance between geometric entities at asserted c
onnectivities');
#2447=UNCERTAINTY_MEASURE_WITH_UNIT(LENGTH_MEASURE(0.01),#2463,
'DISTANCE_ACCURACY_VALUE',
'Maximum model space distance between geometric entities at asserted c
onnectivities');
#2448=UNCERTAINTY_MEASURE_WITH_UNIT(LENGTH_MEASURE(0.01),#2463,
'DISTANCE_ACCURACY_VALUE',
'Maximum model space distance between geometric entities at asserted c
onnectivities');
#2449=UNCERTAINTY_MEASURE_WITH_UNIT(LENGTH_MEASURE(0.01),#2463,
'DISTANCE_ACCURACY_VALUE',
'Maximum model space distance between geometric entities at asserted c
onnectivities');
#2450=UNCERTAINTY_MEASURE_WITH_UNIT(LENGTH_MEASURE(0.01),#2463,
'DISTANCE_ACCURACY_VALUE',
'Maximum model space distance between geometric entities at asserted c
onnectivities');
#2451=UNCERTAINTY_MEASURE_WITH_UNIT(LENGTH_MEASURE(0.01),#2463,
'DISTANCE_ACCURACY_VALUE',
'Maximum model space distance between geometric entities at asserted c
onnectivities');
#2452=(
GEOMETRIC_REPRESENTATION_CONTEXT(3)
GLOBAL_UNCERTAINTY_ASSIGNED_CONTEXT((#2441))
GLOBAL_UNIT_ASSIGNED_CONTEXT((#2463,#2465,#2466))
REPRESENTATION_CONTEXT('','3D')
);
#2453=(
GEOMETRIC_REPRESENTATION_CONTEXT(3)
GLOBAL_UNCERTAINTY_ASSIGNED_CONTEXT((#2442))
GLOBAL_UNIT_ASSIGNED_CONTEXT((#2463,#2465,#2466))
REPRESENTATION_CONTEXT('','3D')
);
#2454=(
GEOMETRIC_REPRESENTATION_CONTEXT(3)
GLOBAL_UNCERTAINTY_ASSIGNED_CONTEXT((#2443))
GLOBAL_UNIT_ASSIGNED_CONTEXT((#2463,#2465,#2466))
REPRESENTATION_CONTEXT('','3D')
);
#2455=(
GEOMETRIC_REPRESENTATION_CONTEXT(3)
GLOBAL_UNCERTAINTY_ASSIGNED_CONTEXT((#2444))
GLOBAL_UNIT_ASSIGNED_CONTEXT((#2463,#2465,#2466))
REPRESENTATION_CONTEXT('','3D')
);
#2456=(
GEOMETRIC_REPRESENTATION_CONTEXT(3)
GLOBAL_UNCERTAINTY_ASSIGNED_CONTEXT((#2445))
GLOBAL_UNIT_ASSIGNED_CONTEXT((#2463,#2465,#2466))
REPRESENTATION_CONTEXT('','3D')
);
#2457=(
GEOMETRIC_REPRESENTATION_CONTEXT(3)
GLOBAL_UNCERTAINTY_ASSIGNED_CONTEXT((#2446))
GLOBAL_UNIT_ASSIGNED_CONTEXT((#2463,#2465,#2466))
REPRESENTATION_CONTEXT('','3D')
);
#2458=(
GEOMETRIC_REPRESENTATION_CONTEXT(3)
GLOBAL_UNCERTAINTY_ASSIGNED_CONTEXT((#2447))
GLOBAL_UNIT_ASSIGNED_CONTEXT((#2463,#2465,#2466))
REPRESENTATION_CONTEXT('','3D')
);
#2459=(
GEOMETRIC_REPRESENTATION_CONTEXT(3)
GLOBAL_UNCERTAINTY_ASSIGNED_CONTEXT((#2448))
GLOBAL_UNIT_ASSIGNED_CONTEXT((#2463,#2465,#2466))
REPRESENTATION_CONTEXT('','3D')
);
#2460=(
GEOMETRIC_REPRESENTATION_CONTEXT(3)
GLOBAL_UNCERTAINTY_ASSIGNED_CONTEXT((#2449))
GLOBAL_UNIT_ASSIGNED_CONTEXT((#2463,#2465,#2466))
REPRESENTATION_CONTEXT('','3D')
);
#2461=(
GEOMETRIC_REPRESENTATION_CONTEXT(3)
GLOBAL_UNCERTAINTY_ASSIGNED_CONTEXT((#2450))
GLOBAL_UNIT_ASSIGNED_CONTEXT((#2463,#2465,#2466))
REPRESENTATION_CONTEXT('','3D')
);
#2462=(
GEOMETRIC_REPRESENTATION_CONTEXT(3)
GLOBAL_UNCERTAINTY_ASSIGNED_CONTEXT((#2451))
GLOBAL_UNIT_ASSIGNED_CONTEXT((#2463,#2465,#2466))
REPRESENTATION_CONTEXT('','3D')
);
#2463=(
LENGTH_UNIT()
NAMED_UNIT(*)
SI_UNIT(.MILLI.,.METRE.)
);
#2464=(
LENGTH_UNIT()
NAMED_UNIT(*)
SI_UNIT($,.METRE.)
);
#2465=(
NAMED_UNIT(*)
PLANE_ANGLE_UNIT()
SI_UNIT($,.RADIAN.)
);
#2466=(
NAMED_UNIT(*)
SI_UNIT($,.STERADIAN.)
SOLID_ANGLE_UNIT()
);
#2467=SHAPE_DEFINITION_REPRESENTATION(#2477,#2497);
#2468=SHAPE_DEFINITION_REPRESENTATION(#2478,#2498);
#2469=SHAPE_DEFINITION_REPRESENTATION(#2479,#2499);
#2470=SHAPE_DEFINITION_REPRESENTATION(#2480,#2500);
#2471=SHAPE_DEFINITION_REPRESENTATION(#2481,#2501);
#2472=SHAPE_DEFINITION_REPRESENTATION(#2482,#2502);
#2473=SHAPE_DEFINITION_REPRESENTATION(#2483,#2503);
#2474=SHAPE_DEFINITION_REPRESENTATION(#2484,#2504);
#2475=SHAPE_DEFINITION_REPRESENTATION(#2485,#2505);
#2476=SHAPE_DEFINITION_REPRESENTATION(#2486,#2506);
#2477=PRODUCT_DEFINITION_SHAPE('',$,#2508);
#2478=PRODUCT_DEFINITION_SHAPE('',$,#2509);
#2479=PRODUCT_DEFINITION_SHAPE('',$,#2510);
#2480=PRODUCT_DEFINITION_SHAPE('',$,#2511);
#2481=PRODUCT_DEFINITION_SHAPE('',$,#2512);
#2482=PRODUCT_DEFINITION_SHAPE('',$,#2513);
#2483=PRODUCT_DEFINITION_SHAPE('',$,#2514);
#2484=PRODUCT_DEFINITION_SHAPE('',$,#2515);
#2485=PRODUCT_DEFINITION_SHAPE('',$,#2516);
#2486=PRODUCT_DEFINITION_SHAPE('',$,#2517);
#2487=PRODUCT_DEFINITION_SHAPE($,$,#41);
#2488=PRODUCT_DEFINITION_SHAPE($,$,#42);
#2489=PRODUCT_DEFINITION_SHAPE($,$,#43);
#2490=PRODUCT_DEFINITION_SHAPE($,$,#44);
#2491=PRODUCT_DEFINITION_SHAPE($,$,#45);
#2492=PRODUCT_DEFINITION_SHAPE($,$,#46);
#2493=PRODUCT_DEFINITION_SHAPE($,$,#47);
#2494=PRODUCT_DEFINITION_SHAPE($,$,#48);
#2495=PRODUCT_DEFINITION_SHAPE($,$,#49);
#2496=PRODUCT_DEFINITION_SHAPE($,$,#50);
#2497=SHAPE_REPRESENTATION('',(#1436,#1569,#1570,#1571,#1572,#1573,#1574,
#1575,#1576,#1577,#1578),#2452);
#2498=SHAPE_REPRESENTATION('',(#1437),#2453);
#2499=SHAPE_REPRESENTATION('',(#1443),#2454);
#2500=SHAPE_REPRESENTATION('',(#1464),#2455);
#2501=SHAPE_REPRESENTATION('',(#1478),#2456);
#2502=SHAPE_REPRESENTATION('',(#1488),#2457);
#2503=SHAPE_REPRESENTATION('',(#1501),#2458);
#2504=SHAPE_REPRESENTATION('',(#1509),#2459);
#2505=SHAPE_REPRESENTATION('',(#1523),#2460);
#2506=SHAPE_REPRESENTATION('',(#1544),#2461);
#2507=PRODUCT_DEFINITION_CONTEXT('part definition',#2539,'design');
#2508=PRODUCT_DEFINITION('BR-205','BR-205',#2518,#2507);
#2509=PRODUCT_DEFINITION('Rod','Rod',#2519,#2507);
#2510=PRODUCT_DEFINITION('Connector_01','Connector_01',#2520,#2507);
#2511=PRODUCT_DEFINITION('Disk','Disk',#2521,#2507);
#2512=PRODUCT_DEFINITION('base','Base',#2522,#2507);
#2513=PRODUCT_DEFINITION('Bar','Bar',#2523,#2507);
#2514=PRODUCT_DEFINITION('Round_Scale','Round_Scale',#2524,#2507);
#2515=PRODUCT_DEFINITION('Shaft','Shaft',#2525,#2507);
#2516=PRODUCT_DEFINITION('Connector_02','Connector_02',#2526,#2507);
#2517=PRODUCT_DEFINITION(
'BSHCS ASME B18.3.1M - M20x2.5 x 20 Steel Grade 2 Plain_1','Screw_02',#2527,
#2507);
#2518=PRODUCT_DEFINITION_FORMATION('',$,#2541);
#2519=PRODUCT_DEFINITION_FORMATION('',$,#2542);
#2520=PRODUCT_DEFINITION_FORMATION('',$,#2543);
#2521=PRODUCT_DEFINITION_FORMATION('',$,#2544);
#2522=PRODUCT_DEFINITION_FORMATION('',$,#2545);
#2523=PRODUCT_DEFINITION_FORMATION('',$,#2546);
#2524=PRODUCT_DEFINITION_FORMATION('',$,#2547);
#2525=PRODUCT_DEFINITION_FORMATION('',$,#2548);
#2526=PRODUCT_DEFINITION_FORMATION('',$,#2549);
#2527=PRODUCT_DEFINITION_FORMATION('',$,#2550);
#2528=PRODUCT_RELATED_PRODUCT_CATEGORY('BR-205','BR-205',(#2541));
#2529=PRODUCT_RELATED_PRODUCT_CATEGORY('Rod','Rod',(#2542));
#2530=PRODUCT_RELATED_PRODUCT_CATEGORY('Connector_01','Connector_01',(#2543));
#2531=PRODUCT_RELATED_PRODUCT_CATEGORY('Disk','Disk',(#2544));
#2532=PRODUCT_RELATED_PRODUCT_CATEGORY('Base','Base',(#2545));
#2533=PRODUCT_RELATED_PRODUCT_CATEGORY('Bar','Bar',(#2546));
#2534=PRODUCT_RELATED_PRODUCT_CATEGORY('Round_Scale','Round_Scale',(#2547));
#2535=PRODUCT_RELATED_PRODUCT_CATEGORY('Shaft','Shaft',(#2548));
#2536=PRODUCT_RELATED_PRODUCT_CATEGORY('Connector_02','Connector_02',(#2549));
#2537=PRODUCT_RELATED_PRODUCT_CATEGORY('Screw_02','Screw_02',(#2550));
#2538=APPLICATION_PROTOCOL_DEFINITION('international standard',
'automotive_design',2009,#2539);
#2539=APPLICATION_CONTEXT(
'Core Data for Automotive Mechanical Design Process');
#2540=PRODUCT_CONTEXT('part definition',#2539,'mechanical');
#2541=PRODUCT('BR-205','BR-205',$,(#2540));
#2542=PRODUCT('Rod','Rod',$,(#2540));
#2543=PRODUCT('Connector_01','Connector_01',$,(#2540));
#2544=PRODUCT('Disk','Disk',$,(#2540));
#2545=PRODUCT('base','Base',$,(#2540));
#2546=PRODUCT('Bar','Bar',$,(#2540));
#2547=PRODUCT('Round_Scale','Round_Scale',$,(#2540));
#2548=PRODUCT('Shaft','Shaft',$,(#2540));
#2549=PRODUCT('Connector_02','Connector_02',$,(#2540));
#2550=PRODUCT(
'BSHCS ASME B18.3.1M - M20x2.5 x 20 Steel Grade 2 Plain_1','Screw_02',
'Broached Hexagon Socket Head Cap Screw ASME B18.3.1M - M20x2.5 x 20',(#2540));
#2551=PRESENTATION_STYLE_ASSIGNMENT((#2554));
#2552=PRESENTATION_STYLE_ASSIGNMENT((#2555));
#2553=PRESENTATION_STYLE_ASSIGNMENT((#2556));
#2554=SURFACE_STYLE_USAGE(.BOTH.,#2557);
#2555=SURFACE_STYLE_USAGE(.BOTH.,#2558);
#2556=SURFACE_STYLE_USAGE(.BOTH.,#2559);
#2557=SURFACE_SIDE_STYLE('',(#2560));
#2558=SURFACE_SIDE_STYLE('',(#2561));
#2559=SURFACE_SIDE_STYLE('',(#2562));
#2560=SURFACE_STYLE_FILL_AREA(#2563);
#2561=SURFACE_STYLE_FILL_AREA(#2564);
#2562=SURFACE_STYLE_FILL_AREA(#2565);
#2563=FILL_AREA_STYLE('Steel - Satin',(#2566));
#2564=FILL_AREA_STYLE('Opaque(160,160,160)',(#2567));
#2565=FILL_AREA_STYLE('Opaque(179,179,179)',(#2568));
#2566=FILL_AREA_STYLE_COLOUR('Steel - Satin',#2569);
#2567=FILL_AREA_STYLE_COLOUR('Opaque(160,160,160)',#2570);
#2568=FILL_AREA_STYLE_COLOUR('Opaque(179,179,179)',#2571);
#2569=COLOUR_RGB('Steel - Satin', 0.09019608, 0.27058824, 0.51372549);
#2570=COLOUR_RGB('Opaque(160,160,160)', 0.09019608, 0.27058824, 0.51372549);
#2571=COLOUR_RGB('Opaque(179,179,179)', 0.31764706, 0.68627451, 0.89019608);
ENDSEC;
END-ISO-10303-21;
